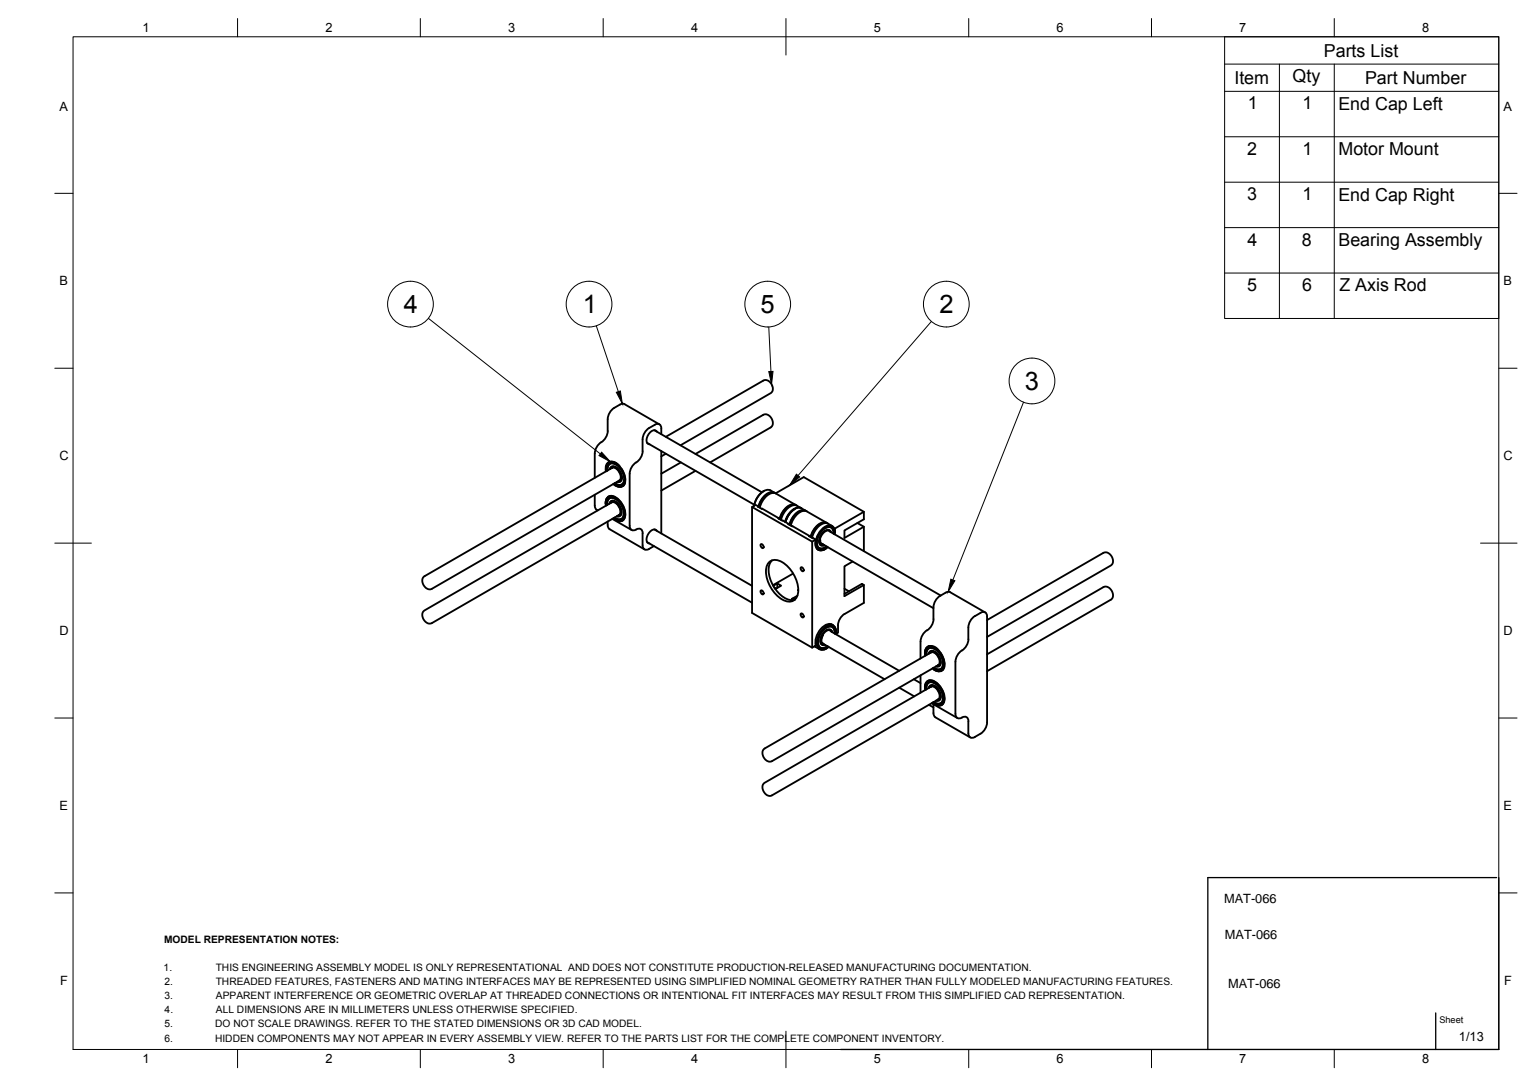
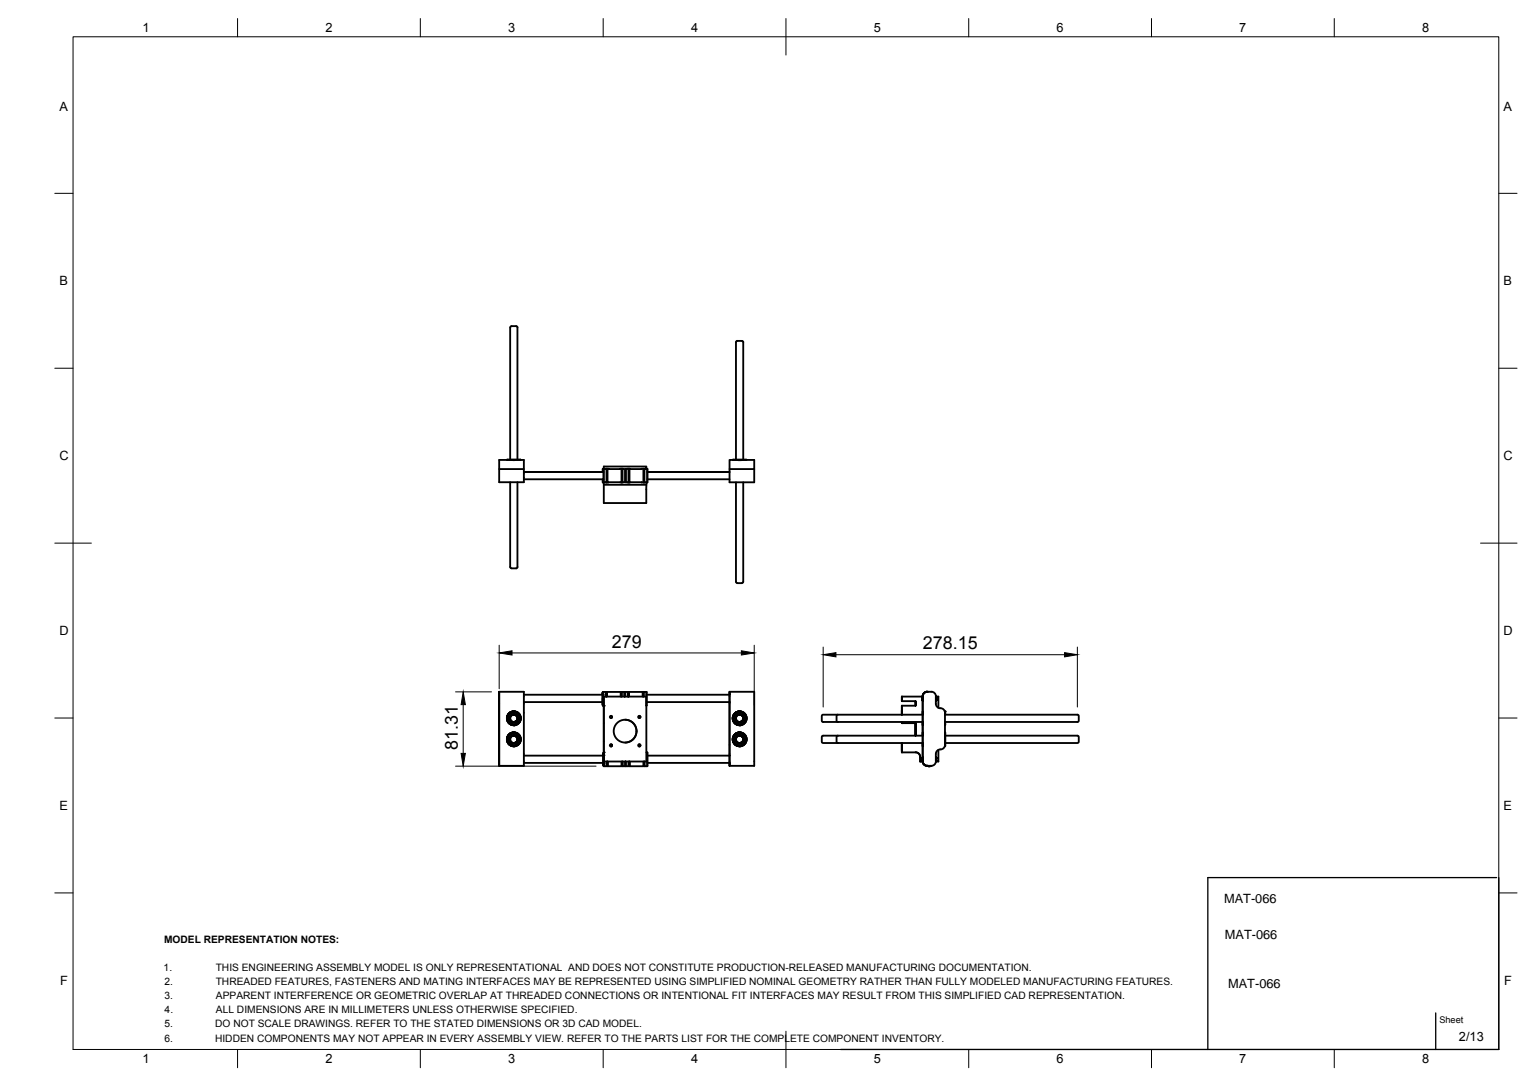
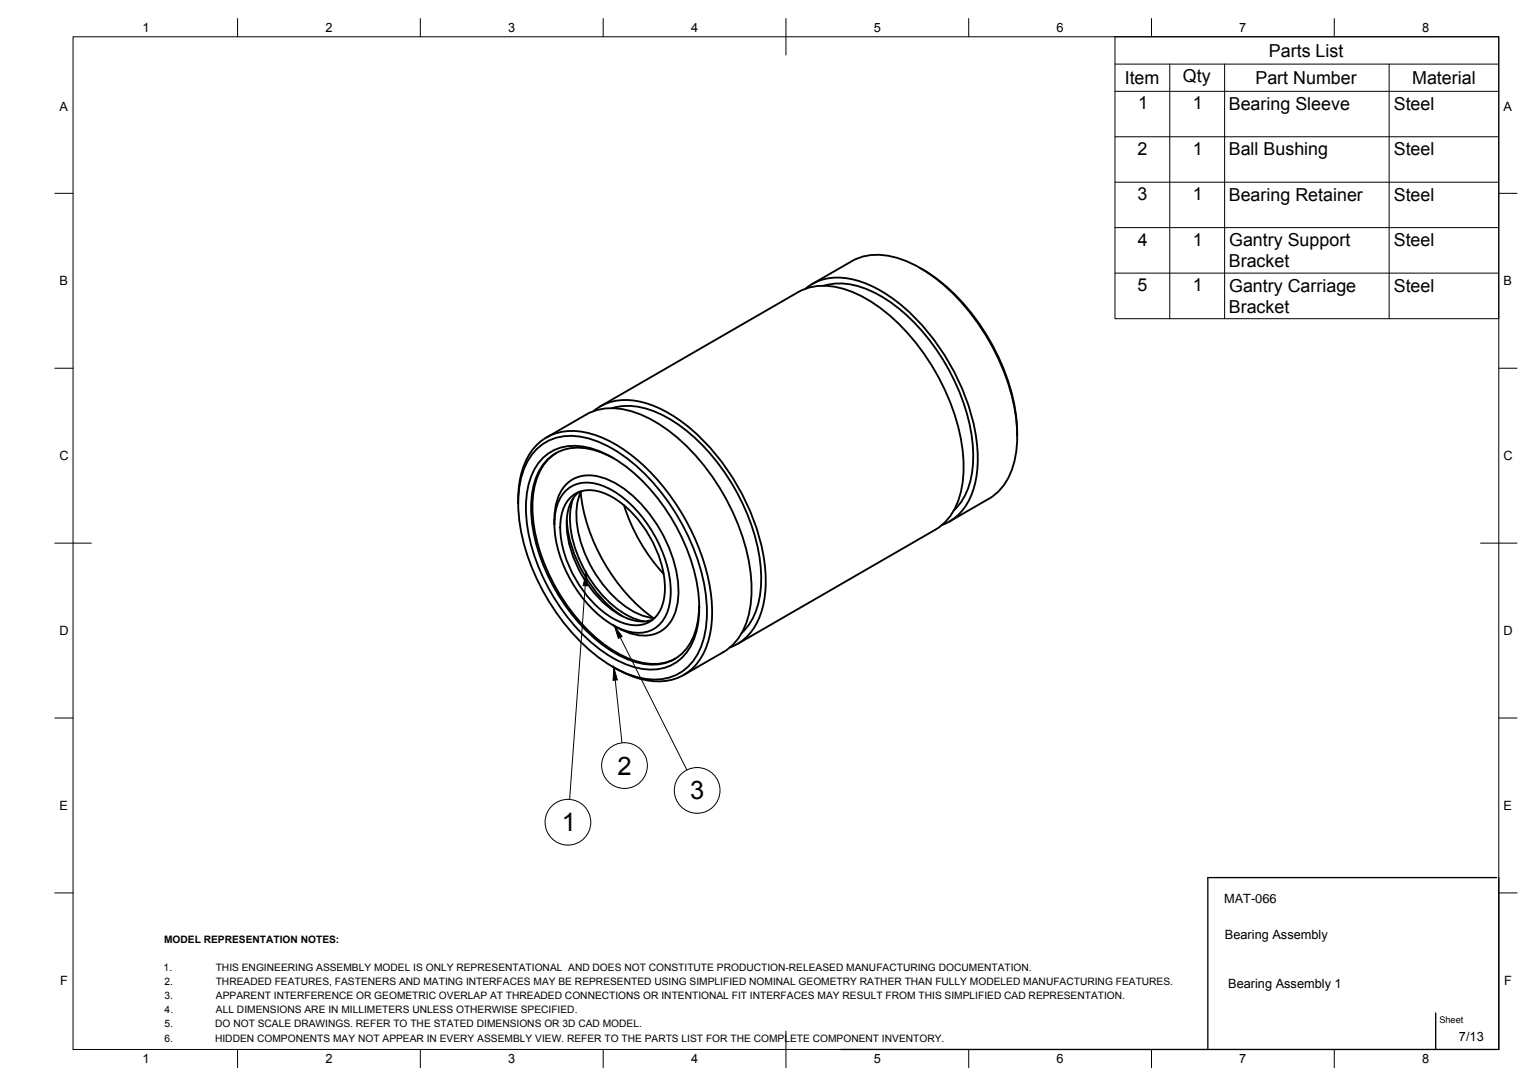
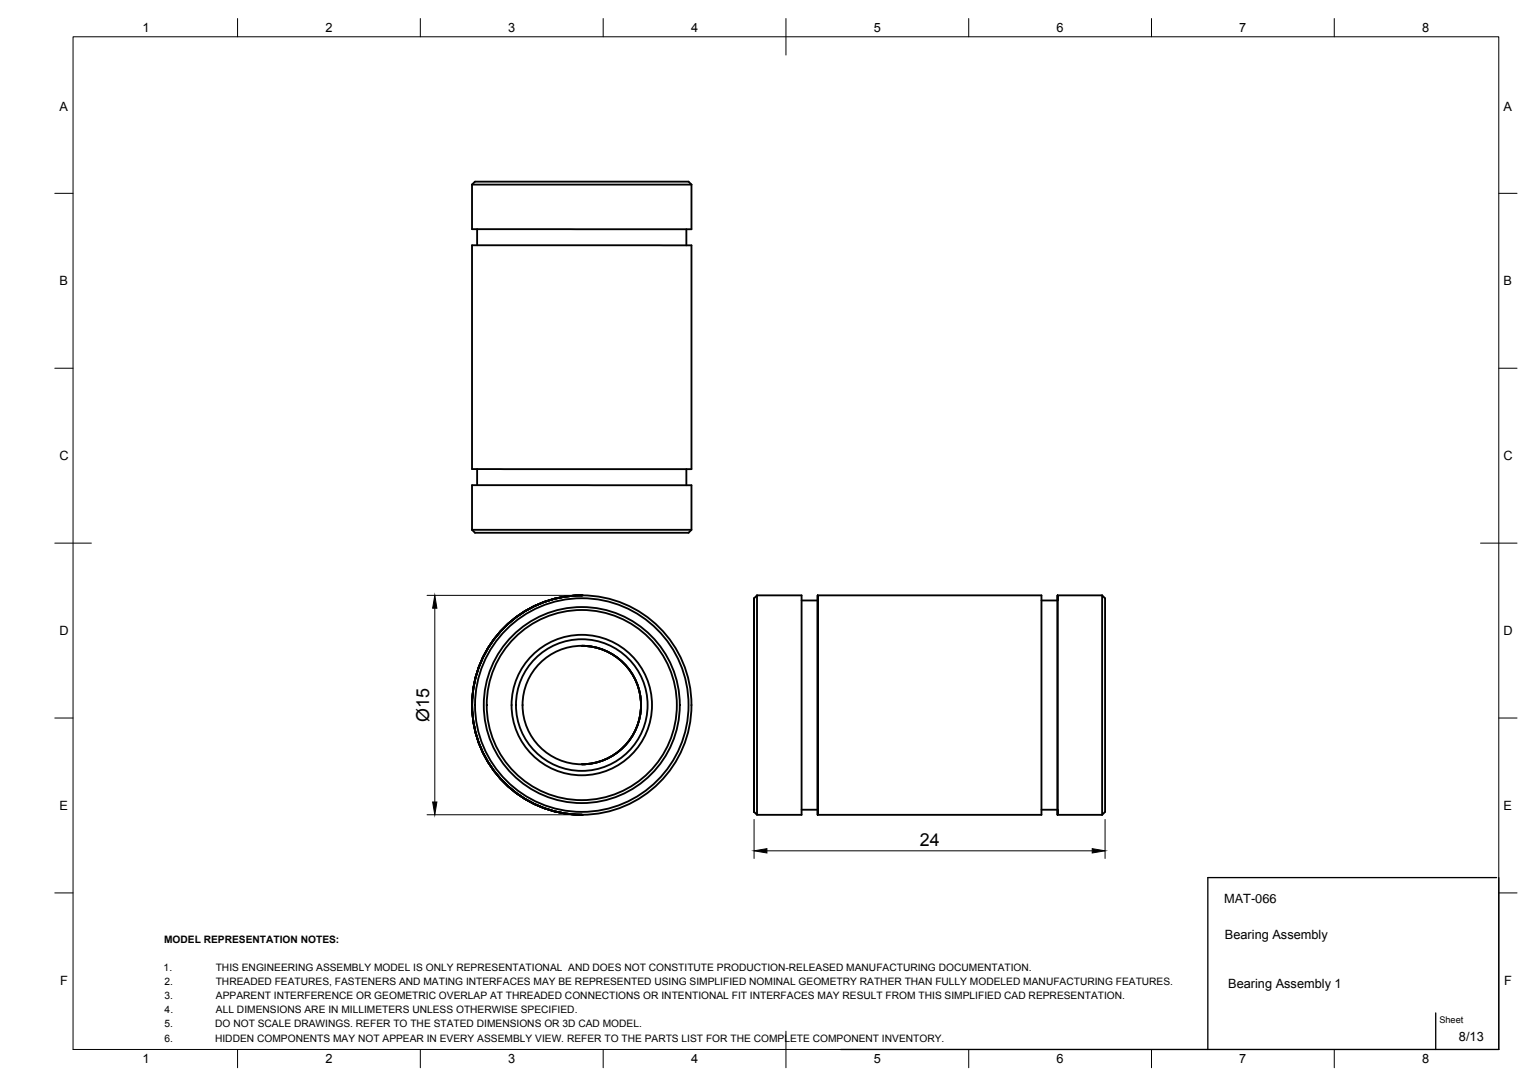
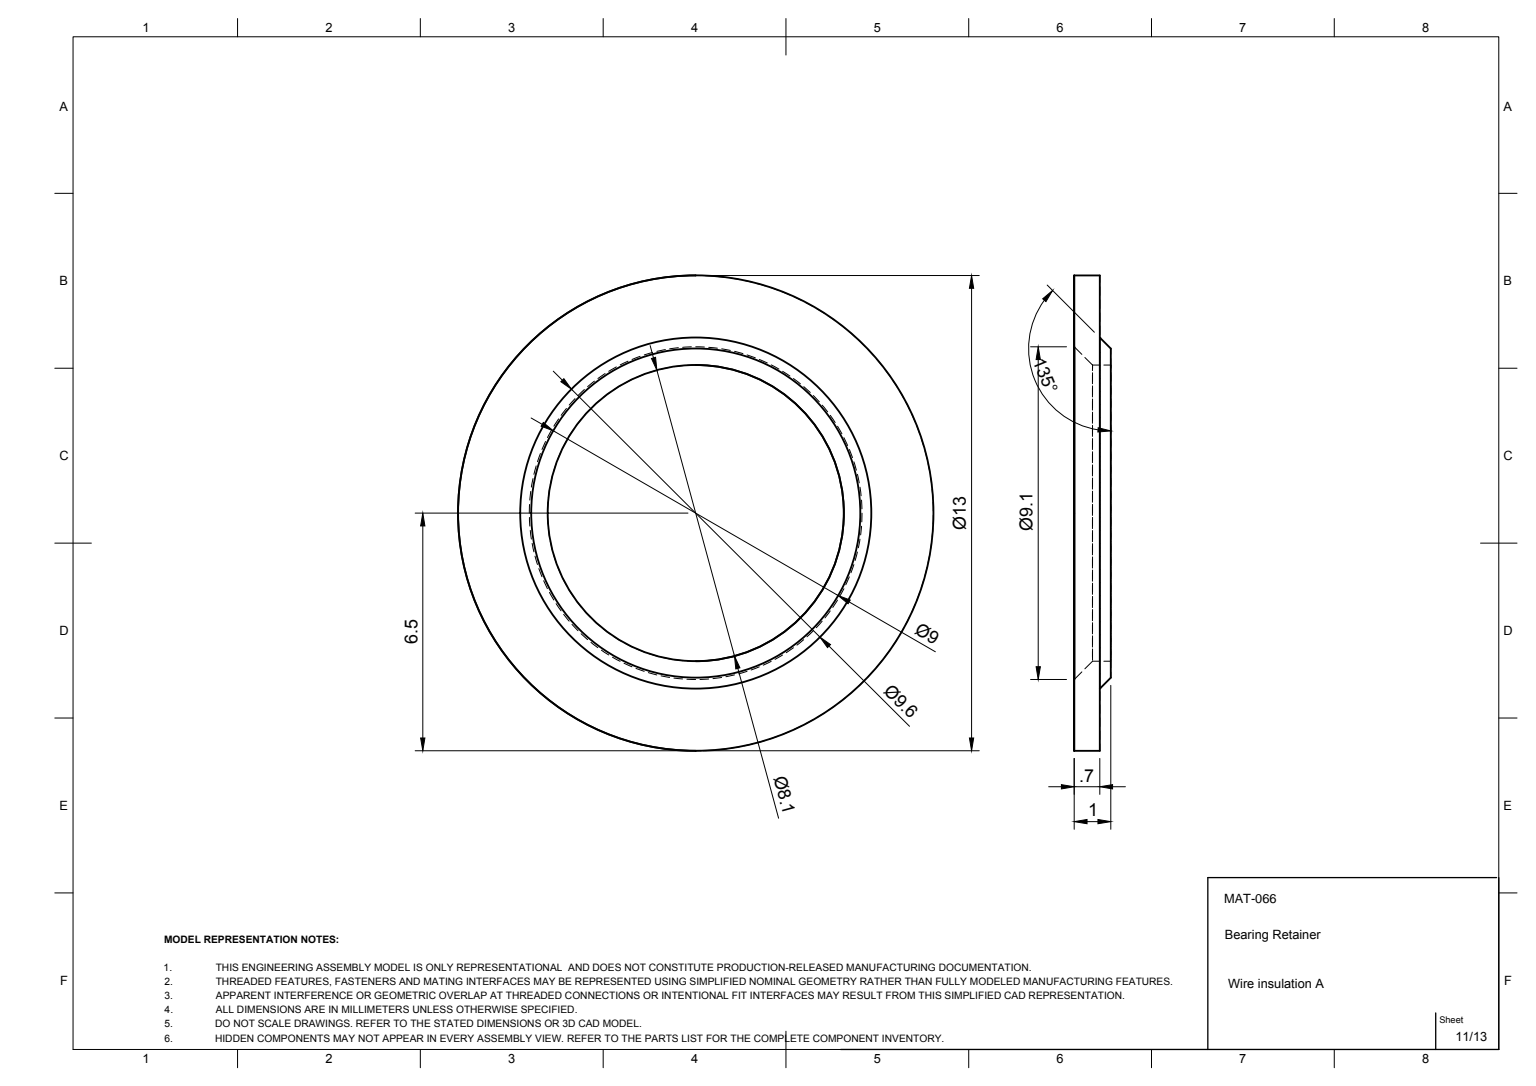
ISO-10303-21;
HEADER;
/* Generated by software containing ST-Developer
 * from STEP Tools, Inc. (www.steptools.com) 
 */

FILE_DESCRIPTION(
/* description */ ('CAx-IF Rec.Pracs.---Representation and Presentation of Product Manufa
cturing Information (PMI)---4.0---2014-10-13'),
/* implementation_level */ '2;1');

FILE_NAME(
/* name */ 'MAT-066',
/* time_stamp */ '2026-10-24T15:58:00-07:00',
/* author */ (''),
/* organization */ (''),
/* preprocessor_version */ 'ST-DEVELOPER v20.2',
/* originating_system */ 'Autodesk Translation Framework v15.17.0.0',
/* authorisation */ '');

FILE_SCHEMA (('AP242_MANAGED_MODEL_BASED_3D_ENGINEERING_MIM_LF { 1 0 10303 442 2 1 4 }'));
ENDSEC;

DATA;
#10=MECHANICAL_DESIGN_GEOMETRIC_PRESENTATION_REPRESENTATION('',(#129,#130,
#131,#132,#133,#134,#135,#136,#137),#8944);
#11=ITEM_DEFINED_TRANSFORMATION($,$,#5686,#5795);
#12=ITEM_DEFINED_TRANSFORMATION($,$,#5695,#5796);
#13=ITEM_DEFINED_TRANSFORMATION($,$,#5756,#5797);
#14=ITEM_DEFINED_TRANSFORMATION($,$,#5771,#5798);
#15=ITEM_DEFINED_TRANSFORMATION($,$,#5780,#5799);
#16=ITEM_DEFINED_TRANSFORMATION($,$,#5260,#5800);
#17=ITEM_DEFINED_TRANSFORMATION($,$,#5308,#5801);
#18=ITEM_DEFINED_TRANSFORMATION($,$,#5623,#5802);
#19=ITEM_DEFINED_TRANSFORMATION($,$,#5685,#5803);
#20=ITEM_DEFINED_TRANSFORMATION($,$,#5671,#5804);
#21=ITEM_DEFINED_TRANSFORMATION($,$,#5671,#5805);
#22=ITEM_DEFINED_TRANSFORMATION($,$,#5671,#5806);
#23=ITEM_DEFINED_TRANSFORMATION($,$,#5671,#5807);
#24=ITEM_DEFINED_TRANSFORMATION($,$,#5671,#5808);
#25=ITEM_DEFINED_TRANSFORMATION($,$,#5671,#5809);
#26=ITEM_DEFINED_TRANSFORMATION($,$,#5685,#5810);
#27=ITEM_DEFINED_TRANSFORMATION($,$,#5685,#5811);
#28=ITEM_DEFINED_TRANSFORMATION($,$,#5685,#5812);
#29=ITEM_DEFINED_TRANSFORMATION($,$,#5685,#5813);
#30=ITEM_DEFINED_TRANSFORMATION($,$,#5685,#5814);
#31=ITEM_DEFINED_TRANSFORMATION($,$,#5685,#5815);
#32=ITEM_DEFINED_TRANSFORMATION($,$,#5685,#5816);
#33=(
REPRESENTATION_RELATIONSHIP($,$,#8998,#8997)
REPRESENTATION_RELATIONSHIP_WITH_TRANSFORMATION(#11)
SHAPE_REPRESENTATION_RELATIONSHIP()
);
#34=(
REPRESENTATION_RELATIONSHIP($,$,#8999,#8997)
REPRESENTATION_RELATIONSHIP_WITH_TRANSFORMATION(#12)
SHAPE_REPRESENTATION_RELATIONSHIP()
);
#35=(
REPRESENTATION_RELATIONSHIP($,$,#9000,#8997)
REPRESENTATION_RELATIONSHIP_WITH_TRANSFORMATION(#13)
SHAPE_REPRESENTATION_RELATIONSHIP()
);
#36=(
REPRESENTATION_RELATIONSHIP($,$,#9001,#8997)
REPRESENTATION_RELATIONSHIP_WITH_TRANSFORMATION(#14)
SHAPE_REPRESENTATION_RELATIONSHIP()
);
#37=(
REPRESENTATION_RELATIONSHIP($,$,#9002,#8997)
REPRESENTATION_RELATIONSHIP_WITH_TRANSFORMATION(#15)
SHAPE_REPRESENTATION_RELATIONSHIP()
);
#38=(
REPRESENTATION_RELATIONSHIP($,$,#8993,#8992)
REPRESENTATION_RELATIONSHIP_WITH_TRANSFORMATION(#16)
SHAPE_REPRESENTATION_RELATIONSHIP()
);
#39=(
REPRESENTATION_RELATIONSHIP($,$,#8994,#8992)
REPRESENTATION_RELATIONSHIP_WITH_TRANSFORMATION(#17)
SHAPE_REPRESENTATION_RELATIONSHIP()
);
#40=(
REPRESENTATION_RELATIONSHIP($,$,#8995,#8992)
REPRESENTATION_RELATIONSHIP_WITH_TRANSFORMATION(#18)
SHAPE_REPRESENTATION_RELATIONSHIP()
);
#41=(
REPRESENTATION_RELATIONSHIP($,$,#8997,#8992)
REPRESENTATION_RELATIONSHIP_WITH_TRANSFORMATION(#19)
SHAPE_REPRESENTATION_RELATIONSHIP()
);
#42=(
REPRESENTATION_RELATIONSHIP($,$,#8996,#8992)
REPRESENTATION_RELATIONSHIP_WITH_TRANSFORMATION(#20)
SHAPE_REPRESENTATION_RELATIONSHIP()
);
#43=(
REPRESENTATION_RELATIONSHIP($,$,#8996,#8992)
REPRESENTATION_RELATIONSHIP_WITH_TRANSFORMATION(#21)
SHAPE_REPRESENTATION_RELATIONSHIP()
);
#44=(
REPRESENTATION_RELATIONSHIP($,$,#8996,#8992)
REPRESENTATION_RELATIONSHIP_WITH_TRANSFORMATION(#22)
SHAPE_REPRESENTATION_RELATIONSHIP()
);
#45=(
REPRESENTATION_RELATIONSHIP($,$,#8996,#8992)
REPRESENTATION_RELATIONSHIP_WITH_TRANSFORMATION(#23)
SHAPE_REPRESENTATION_RELATIONSHIP()
);
#46=(
REPRESENTATION_RELATIONSHIP($,$,#8996,#8992)
REPRESENTATION_RELATIONSHIP_WITH_TRANSFORMATION(#24)
SHAPE_REPRESENTATION_RELATIONSHIP()
);
#47=(
REPRESENTATION_RELATIONSHIP($,$,#8996,#8992)
REPRESENTATION_RELATIONSHIP_WITH_TRANSFORMATION(#25)
SHAPE_REPRESENTATION_RELATIONSHIP()
);
#48=(
REPRESENTATION_RELATIONSHIP($,$,#8997,#8992)
REPRESENTATION_RELATIONSHIP_WITH_TRANSFORMATION(#26)
SHAPE_REPRESENTATION_RELATIONSHIP()
);
#49=(
REPRESENTATION_RELATIONSHIP($,$,#8997,#8992)
REPRESENTATION_RELATIONSHIP_WITH_TRANSFORMATION(#27)
SHAPE_REPRESENTATION_RELATIONSHIP()
);
#50=(
REPRESENTATION_RELATIONSHIP($,$,#8997,#8992)
REPRESENTATION_RELATIONSHIP_WITH_TRANSFORMATION(#28)
SHAPE_REPRESENTATION_RELATIONSHIP()
);
#51=(
REPRESENTATION_RELATIONSHIP($,$,#8997,#8992)
REPRESENTATION_RELATIONSHIP_WITH_TRANSFORMATION(#29)
SHAPE_REPRESENTATION_RELATIONSHIP()
);
#52=(
REPRESENTATION_RELATIONSHIP($,$,#8997,#8992)
REPRESENTATION_RELATIONSHIP_WITH_TRANSFORMATION(#30)
SHAPE_REPRESENTATION_RELATIONSHIP()
);
#53=(
REPRESENTATION_RELATIONSHIP($,$,#8997,#8992)
REPRESENTATION_RELATIONSHIP_WITH_TRANSFORMATION(#31)
SHAPE_REPRESENTATION_RELATIONSHIP()
);
#54=(
REPRESENTATION_RELATIONSHIP($,$,#8997,#8992)
REPRESENTATION_RELATIONSHIP_WITH_TRANSFORMATION(#32)
SHAPE_REPRESENTATION_RELATIONSHIP()
);
#55=CONTEXT_DEPENDENT_SHAPE_REPRESENTATION(#33,#8970);
#56=CONTEXT_DEPENDENT_SHAPE_REPRESENTATION(#34,#8971);
#57=CONTEXT_DEPENDENT_SHAPE_REPRESENTATION(#35,#8972);
#58=CONTEXT_DEPENDENT_SHAPE_REPRESENTATION(#36,#8973);
#59=CONTEXT_DEPENDENT_SHAPE_REPRESENTATION(#37,#8974);
#60=CONTEXT_DEPENDENT_SHAPE_REPRESENTATION(#38,#8975);
#61=CONTEXT_DEPENDENT_SHAPE_REPRESENTATION(#39,#8976);
#62=CONTEXT_DEPENDENT_SHAPE_REPRESENTATION(#40,#8977);
#63=CONTEXT_DEPENDENT_SHAPE_REPRESENTATION(#41,#8978);
#64=CONTEXT_DEPENDENT_SHAPE_REPRESENTATION(#42,#8979);
#65=CONTEXT_DEPENDENT_SHAPE_REPRESENTATION(#43,#8980);
#66=CONTEXT_DEPENDENT_SHAPE_REPRESENTATION(#44,#8981);
#67=CONTEXT_DEPENDENT_SHAPE_REPRESENTATION(#45,#8982);
#68=CONTEXT_DEPENDENT_SHAPE_REPRESENTATION(#46,#8983);
#69=CONTEXT_DEPENDENT_SHAPE_REPRESENTATION(#47,#8984);
#70=CONTEXT_DEPENDENT_SHAPE_REPRESENTATION(#48,#8985);
#71=CONTEXT_DEPENDENT_SHAPE_REPRESENTATION(#49,#8986);
#72=CONTEXT_DEPENDENT_SHAPE_REPRESENTATION(#50,#8987);
#73=CONTEXT_DEPENDENT_SHAPE_REPRESENTATION(#51,#8988);
#74=CONTEXT_DEPENDENT_SHAPE_REPRESENTATION(#52,#8989);
#75=CONTEXT_DEPENDENT_SHAPE_REPRESENTATION(#53,#8990);
#76=CONTEXT_DEPENDENT_SHAPE_REPRESENTATION(#54,#8991);
#77=NEXT_ASSEMBLY_USAGE_OCCURRENCE('Bearing Sleeve:1',
'Bearing Sleeve:1','Bearing Sleeve:1',#9009,#9010,'Bearing Sleeve:1');
#78=NEXT_ASSEMBLY_USAGE_OCCURRENCE('Ball Bushing:1','Ball Bushing:1',
'Ball Bushing:1',#9009,#9011,'Ball Bushing:1');
#79=NEXT_ASSEMBLY_USAGE_OCCURRENCE('Bearing Retainer 1:1',
'Bearing Retainer 1:1','Bearing Retainer 1:1',#9009,#9012,
'Bearing Retainer 1:1');
#80=NEXT_ASSEMBLY_USAGE_OCCURRENCE('Gantry Support Bracket:1',
'Gantry Support Bracket:1','Gantry Support Bracket:1',#9009,#9013,
'Gantry Support Bracket:1');
#81=NEXT_ASSEMBLY_USAGE_OCCURRENCE('Gantry Carriage Bracket:1',
'Gantry Carriage Bracket:1','Gantry Carriage Bracket:1',#9009,#9014,
'Gantry Carriage Bracket:1');
#82=NEXT_ASSEMBLY_USAGE_OCCURRENCE('End Cap Left:1','End Cap Left:1',
'End Cap Left:1',#9004,#9005,'End Cap Left:1');
#83=NEXT_ASSEMBLY_USAGE_OCCURRENCE('Motor Mount:1','Motor Mount:1',
'Motor Mount:1',#9004,#9006,'Motor Mount:1');
#84=NEXT_ASSEMBLY_USAGE_OCCURRENCE('End Cap Right:1','End Cap Right:1',
'End Cap Right:1',#9004,#9007,'End Cap Right:1');
#85=NEXT_ASSEMBLY_USAGE_OCCURRENCE('Bearing Assembly 1:1',
'Bearing Assembly 1:1','Bearing Assembly 1:1',#9004,#9009,
'Bearing Assembly 1:1');
#86=NEXT_ASSEMBLY_USAGE_OCCURRENCE('Z Axis Rod:1','Z Axis Rod:1',
'Z Axis Rod:1',#9004,#9008,'Z Axis Rod:1');
#87=NEXT_ASSEMBLY_USAGE_OCCURRENCE('Z Axis Rod:2','Z Axis Rod:2',
'Z Axis Rod:2',#9004,#9008,'Z Axis Rod:2');
#88=NEXT_ASSEMBLY_USAGE_OCCURRENCE('Z Axis Rod:3','Z Axis Rod:3',
'Z Axis Rod:3',#9004,#9008,'Z Axis Rod:3');
#89=NEXT_ASSEMBLY_USAGE_OCCURRENCE('Z Axis Rod:4','Z Axis Rod:4',
'Z Axis Rod:4',#9004,#9008,'Z Axis Rod:4');
#90=NEXT_ASSEMBLY_USAGE_OCCURRENCE('Z Axis Rod:5','Z Axis Rod:5',
'Z Axis Rod:5',#9004,#9008,'Z Axis Rod:5');
#91=NEXT_ASSEMBLY_USAGE_OCCURRENCE('Z Axis Rod:6','Z Axis Rod:6',
'Z Axis Rod:6',#9004,#9008,'Z Axis Rod:6');
#92=NEXT_ASSEMBLY_USAGE_OCCURRENCE('Bearing Assembly 1:2',
'Bearing Assembly 1:2','Bearing Assembly 1:2',#9004,#9009,
'Bearing Assembly 1:2');
#93=NEXT_ASSEMBLY_USAGE_OCCURRENCE('Bearing Assembly 1:3',
'Bearing Assembly 1:3','Bearing Assembly 1:3',#9004,#9009,
'Bearing Assembly 1:3');
#94=NEXT_ASSEMBLY_USAGE_OCCURRENCE('Bearing Assembly 1:4',
'Bearing Assembly 1:4','Bearing Assembly 1:4',#9004,#9009,
'Bearing Assembly 1:4');
#95=NEXT_ASSEMBLY_USAGE_OCCURRENCE('Bearing Assembly 1:5',
'Bearing Assembly 1:5','Bearing Assembly 1:5',#9004,#9009,
'Bearing Assembly 1:5');
#96=NEXT_ASSEMBLY_USAGE_OCCURRENCE('Bearing Assembly 1:6',
'Bearing Assembly 1:6','Bearing Assembly 1:6',#9004,#9009,
'Bearing Assembly 1:6');
#97=NEXT_ASSEMBLY_USAGE_OCCURRENCE('Bearing Assembly 1:7',
'Bearing Assembly 1:7','Bearing Assembly 1:7',#9004,#9009,
'Bearing Assembly 1:7');
#98=NEXT_ASSEMBLY_USAGE_OCCURRENCE('Bearing Assembly 1:8',
'Bearing Assembly 1:8','Bearing Assembly 1:8',#9004,#9009,
'Bearing Assembly 1:8');
#99=CONICAL_SURFACE('',#5696,0.0066,0.785398163397459);
#100=CONICAL_SURFACE('',#5704,0.0074,0.785398163397448);
#101=CONICAL_SURFACE('',#5709,0.0066,0.785398163397459);
#102=CONICAL_SURFACE('',#5717,0.0074,0.785398163397448);
#103=CONICAL_SURFACE('',#5730,0.0061,0.158655262186402);
#104=CONICAL_SURFACE('',#5734,0.0061,0.158655262186402);
#105=CONICAL_SURFACE('',#5764,0.0043,0.785398163397448);
#106=CONICAL_SURFACE('',#5770,0.0046499998960644,0.785398163397448);
#107=CONICAL_SURFACE('',#5788,0.0043,0.785398163397448);
#108=CONICAL_SURFACE('',#5794,0.0046499998960644,0.785398163397448);
#109=TOROIDAL_SURFACE('',#5681,0.0025,0.0015);
#110=TOROIDAL_SURFACE('',#5683,0.0025,0.0015);
#111=SHAPE_REPRESENTATION_RELATIONSHIP('SRR','None',#8993,#120);
#112=SHAPE_REPRESENTATION_RELATIONSHIP('SRR','None',#8994,#121);
#113=SHAPE_REPRESENTATION_RELATIONSHIP('SRR','None',#8995,#122);
#114=SHAPE_REPRESENTATION_RELATIONSHIP('SRR','None',#8996,#123);
#115=SHAPE_REPRESENTATION_RELATIONSHIP('SRR','None',#8998,#124);
#116=SHAPE_REPRESENTATION_RELATIONSHIP('SRR','None',#8999,#125);
#117=SHAPE_REPRESENTATION_RELATIONSHIP('SRR','None',#9000,#126);
#118=SHAPE_REPRESENTATION_RELATIONSHIP('SRR','None',#9001,#127);
#119=SHAPE_REPRESENTATION_RELATIONSHIP('SRR','None',#9002,#128);
#120=ADVANCED_BREP_SHAPE_REPRESENTATION('',(#138),#8934);
#121=ADVANCED_BREP_SHAPE_REPRESENTATION('',(#139),#8935);
#122=ADVANCED_BREP_SHAPE_REPRESENTATION('',(#140),#8936);
#123=ADVANCED_BREP_SHAPE_REPRESENTATION('',(#141),#8937);
#124=ADVANCED_BREP_SHAPE_REPRESENTATION('',(#142),#8939);
#125=ADVANCED_BREP_SHAPE_REPRESENTATION('',(#143),#8940);
#126=ADVANCED_BREP_SHAPE_REPRESENTATION('',(#144),#8941);
#127=ADVANCED_BREP_SHAPE_REPRESENTATION('',(#145),#8942);
#128=ADVANCED_BREP_SHAPE_REPRESENTATION('',(#146),#8943);
#129=STYLED_ITEM('',(#9052),#138);
#130=STYLED_ITEM('',(#9053),#139);
#131=STYLED_ITEM('',(#9054),#140);
#132=STYLED_ITEM('',(#9055),#141);
#133=STYLED_ITEM('',(#9052),#142);
#134=STYLED_ITEM('',(#9054),#143);
#135=STYLED_ITEM('',(#9052),#144);
#136=STYLED_ITEM('',(#9054),#145);
#137=STYLED_ITEM('',(#9052),#146);
#138=MANIFOLD_SOLID_BREP('Body1',#5150);
#139=MANIFOLD_SOLID_BREP('Body1',#5151);
#140=MANIFOLD_SOLID_BREP('Body1',#5152);
#141=MANIFOLD_SOLID_BREP('Body1',#5153);
#142=MANIFOLD_SOLID_BREP('Body1',#5154);
#143=MANIFOLD_SOLID_BREP('Body1',#5155);
#144=MANIFOLD_SOLID_BREP('Body1',#5156);
#145=MANIFOLD_SOLID_BREP('Body1',#5157);
#146=MANIFOLD_SOLID_BREP('Body1',#5158);
#147=B_SPLINE_CURVE_WITH_KNOTS('',3,(#7501,#7502,#7503,#7504,#7505,#7506),
 .UNSPECIFIED.,.F.,.F.,(4,2,4),(3.46797062946804,3.66737221611079,3.95578831781598),
 .UNSPECIFIED.);
#148=B_SPLINE_CURVE_WITH_KNOTS('',3,(#7507,#7508,#7509,#7510,#7511,#7512),
 .UNSPECIFIED.,.F.,.F.,(4,2,4),(3.95578831781598,4.24420441952117,4.44360600616391),
 .UNSPECIFIED.);
#149=B_SPLINE_CURVE_WITH_KNOTS('',3,(#7515,#7516,#7517,#7518,#7519,#7520,
#7521,#7522,#7523,#7524),.UNSPECIFIED.,.F.,.F.,(4,2,2,2,4),(-4.44360600616391,
-4.24420441952117,-3.95578831781597,-3.66737221611078,-3.46797062946804),
 .UNSPECIFIED.);
#150=B_SPLINE_CURVE_WITH_KNOTS('',3,(#8654,#8655,#8656,#8657,#8658,#8659),
 .UNSPECIFIED.,.F.,.F.,(4,2,4),(3.46797062946804,3.66737221611079,3.95578831781598),
 .UNSPECIFIED.);
#151=B_SPLINE_CURVE_WITH_KNOTS('',3,(#8660,#8661,#8662,#8663,#8664,#8665),
 .UNSPECIFIED.,.F.,.F.,(4,2,4),(3.95578831781598,4.24420441952117,4.44360600616391),
 .UNSPECIFIED.);
#152=B_SPLINE_CURVE_WITH_KNOTS('',3,(#8668,#8669,#8670,#8671,#8672,#8673,
#8674,#8675,#8676,#8677),.UNSPECIFIED.,.F.,.F.,(4,2,2,2,4),(3.46797062946804,
3.66737221611078,3.95578831781597,4.24420441952117,4.44360600616391),
 .UNSPECIFIED.);
#153=CYLINDRICAL_SURFACE('',#5276,0.004225);
#154=CYLINDRICAL_SURFACE('',#5280,0.004225);
#155=CYLINDRICAL_SURFACE('',#5294,0.005);
#156=CYLINDRICAL_SURFACE('',#5295,0.005);
#157=CYLINDRICAL_SURFACE('',#5296,0.005);
#158=CYLINDRICAL_SURFACE('',#5297,0.005);
#159=CYLINDRICAL_SURFACE('',#5302,0.007625);
#160=CYLINDRICAL_SURFACE('',#5303,0.007625);
#161=CYLINDRICAL_SURFACE('',#5304,0.005);
#162=CYLINDRICAL_SURFACE('',#5305,0.005);
#163=CYLINDRICAL_SURFACE('',#5306,0.005);
#164=CYLINDRICAL_SURFACE('',#5307,0.005);
#165=CYLINDRICAL_SURFACE('',#5384,0.0125);
#166=CYLINDRICAL_SURFACE('',#5385,0.00123);
#167=CYLINDRICAL_SURFACE('',#5386,0.00123);
#168=CYLINDRICAL_SURFACE('',#5387,0.00123);
#169=CYLINDRICAL_SURFACE('',#5388,0.00123);
#170=CYLINDRICAL_SURFACE('',#5414,0.0076);
#171=CYLINDRICAL_SURFACE('',#5487,0.0023);
#172=CYLINDRICAL_SURFACE('',#5488,0.0023);
#173=CYLINDRICAL_SURFACE('',#5489,0.0023);
#174=CYLINDRICAL_SURFACE('',#5490,0.0023);
#175=CYLINDRICAL_SURFACE('',#5491,0.0023);
#176=CYLINDRICAL_SURFACE('',#5492,0.0023);
#177=CYLINDRICAL_SURFACE('',#5493,0.0023);
#178=CYLINDRICAL_SURFACE('',#5494,0.0023);
#179=CYLINDRICAL_SURFACE('',#5495,0.0023);
#180=CYLINDRICAL_SURFACE('',#5496,0.0023);
#181=CYLINDRICAL_SURFACE('',#5497,0.0023);
#182=CYLINDRICAL_SURFACE('',#5498,0.0023);
#183=CYLINDRICAL_SURFACE('',#5499,0.0023);
#184=CYLINDRICAL_SURFACE('',#5500,0.0023);
#185=CYLINDRICAL_SURFACE('',#5501,0.0023);
#186=CYLINDRICAL_SURFACE('',#5502,0.0023);
#187=CYLINDRICAL_SURFACE('',#5525,0.0076);
#188=CYLINDRICAL_SURFACE('',#5606,0.0023);
#189=CYLINDRICAL_SURFACE('',#5607,0.0023);
#190=CYLINDRICAL_SURFACE('',#5608,0.0023);
#191=CYLINDRICAL_SURFACE('',#5609,0.0023);
#192=CYLINDRICAL_SURFACE('',#5610,0.0023);
#193=CYLINDRICAL_SURFACE('',#5611,0.0023);
#194=CYLINDRICAL_SURFACE('',#5612,0.0023);
#195=CYLINDRICAL_SURFACE('',#5613,0.0023);
#196=CYLINDRICAL_SURFACE('',#5614,0.0023);
#197=CYLINDRICAL_SURFACE('',#5615,0.0023);
#198=CYLINDRICAL_SURFACE('',#5616,0.0023);
#199=CYLINDRICAL_SURFACE('',#5617,0.0023);
#200=CYLINDRICAL_SURFACE('',#5618,0.0023);
#201=CYLINDRICAL_SURFACE('',#5619,0.0023);
#202=CYLINDRICAL_SURFACE('',#5620,0.0023);
#203=CYLINDRICAL_SURFACE('',#5621,0.0023);
#204=CYLINDRICAL_SURFACE('',#5622,0.005);
#205=CYLINDRICAL_SURFACE('',#5639,0.004225);
#206=CYLINDRICAL_SURFACE('',#5643,0.004225);
#207=CYLINDRICAL_SURFACE('',#5657,0.005);
#208=CYLINDRICAL_SURFACE('',#5658,0.005);
#209=CYLINDRICAL_SURFACE('',#5659,0.005);
#210=CYLINDRICAL_SURFACE('',#5660,0.005);
#211=CYLINDRICAL_SURFACE('',#5665,0.007625);
#212=CYLINDRICAL_SURFACE('',#5666,0.007625);
#213=CYLINDRICAL_SURFACE('',#5667,0.005);
#214=CYLINDRICAL_SURFACE('',#5668,0.005);
#215=CYLINDRICAL_SURFACE('',#5669,0.005);
#216=CYLINDRICAL_SURFACE('',#5670,0.005);
#217=CYLINDRICAL_SURFACE('',#5672,0.004);
#218=CYLINDRICAL_SURFACE('',#5690,0.007);
#219=CYLINDRICAL_SURFACE('',#5694,0.0043);
#220=CYLINDRICAL_SURFACE('',#5702,0.0065);
#221=CYLINDRICAL_SURFACE('',#5707,0.0075);
#222=CYLINDRICAL_SURFACE('',#5715,0.0065);
#223=CYLINDRICAL_SURFACE('',#5720,0.0075);
#224=CYLINDRICAL_SURFACE('',#5724,0.00700000010430813);
#225=CYLINDRICAL_SURFACE('',#5728,0.0063);
#226=CYLINDRICAL_SURFACE('',#5732,0.0059);
#227=CYLINDRICAL_SURFACE('',#5736,0.0063);
#228=CYLINDRICAL_SURFACE('',#5740,0.00700000010430813);
#229=CYLINDRICAL_SURFACE('',#5745,0.00715);
#230=CYLINDRICAL_SURFACE('',#5749,0.0075);
#231=CYLINDRICAL_SURFACE('',#5753,0.00715);
#232=CYLINDRICAL_SURFACE('',#5760,0.0065);
#233=CYLINDRICAL_SURFACE('',#5766,0.00405);
#234=CYLINDRICAL_SURFACE('',#5775,0.007);
#235=CYLINDRICAL_SURFACE('',#5779,0.0043);
#236=CYLINDRICAL_SURFACE('',#5784,0.0065);
#237=CYLINDRICAL_SURFACE('',#5790,0.00405);
#238=FACE_BOUND('',#581,.T.);
#239=FACE_BOUND('',#582,.T.);
#240=FACE_BOUND('',#588,.T.);
#241=FACE_BOUND('',#589,.T.);
#242=FACE_BOUND('',#613,.T.);
#243=FACE_BOUND('',#614,.T.);
#244=FACE_BOUND('',#615,.T.);
#245=FACE_BOUND('',#616,.T.);
#246=FACE_BOUND('',#617,.T.);
#247=FACE_BOUND('',#618,.T.);
#248=FACE_BOUND('',#619,.T.);
#249=FACE_BOUND('',#620,.T.);
#250=FACE_BOUND('',#634,.T.);
#251=FACE_BOUND('',#635,.T.);
#252=FACE_BOUND('',#636,.T.);
#253=FACE_BOUND('',#637,.T.);
#254=FACE_BOUND('',#638,.T.);
#255=FACE_BOUND('',#639,.T.);
#256=FACE_BOUND('',#640,.T.);
#257=FACE_BOUND('',#641,.T.);
#258=FACE_BOUND('',#659,.T.);
#259=FACE_BOUND('',#660,.T.);
#260=FACE_BOUND('',#661,.T.);
#261=FACE_BOUND('',#662,.T.);
#262=FACE_BOUND('',#663,.T.);
#263=FACE_BOUND('',#666,.T.);
#264=FACE_BOUND('',#667,.T.);
#265=FACE_BOUND('',#668,.T.);
#266=FACE_BOUND('',#669,.T.);
#267=FACE_BOUND('',#670,.T.);
#268=FACE_BOUND('',#694,.T.);
#269=FACE_BOUND('',#695,.T.);
#270=FACE_BOUND('',#696,.T.);
#271=FACE_BOUND('',#697,.T.);
#272=FACE_BOUND('',#698,.T.);
#273=FACE_BOUND('',#699,.T.);
#274=FACE_BOUND('',#700,.T.);
#275=FACE_BOUND('',#701,.T.);
#276=FACE_BOUND('',#758,.T.);
#277=FACE_BOUND('',#759,.T.);
#278=FACE_BOUND('',#760,.T.);
#279=FACE_BOUND('',#761,.T.);
#280=FACE_BOUND('',#762,.T.);
#281=FACE_BOUND('',#763,.T.);
#282=FACE_BOUND('',#764,.T.);
#283=FACE_BOUND('',#765,.T.);
#284=FACE_BOUND('',#819,.T.);
#285=FACE_BOUND('',#820,.T.);
#286=FACE_BOUND('',#826,.T.);
#287=FACE_BOUND('',#827,.T.);
#288=FACE_BOUND('',#847,.T.);
#289=FACE_BOUND('',#850,.T.);
#290=FACE_BOUND('',#854,.T.);
#291=FACE_BOUND('',#860,.T.);
#292=FACE_BOUND('',#865,.T.);
#293=FACE_BOUND('',#868,.T.);
#294=FACE_BOUND('',#875,.T.);
#295=FACE_BOUND('',#878,.T.);
#296=FACE_BOUND('',#880,.T.);
#297=FACE_BOUND('',#883,.T.);
#298=FACE_BOUND('',#886,.T.);
#299=FACE_BOUND('',#889,.T.);
#300=FACE_BOUND('',#891,.T.);
#301=FACE_BOUND('',#894,.T.);
#302=FACE_BOUND('',#898,.T.);
#303=FACE_BOUND('',#901,.T.);
#304=FACE_BOUND('',#904,.T.);
#305=FACE_BOUND('',#907,.T.);
#306=FACE_BOUND('',#910,.T.);
#307=FACE_BOUND('',#914,.T.);
#308=FACE_OUTER_BOUND('',#577,.T.);
#309=FACE_OUTER_BOUND('',#578,.T.);
#310=FACE_OUTER_BOUND('',#579,.T.);
#311=FACE_OUTER_BOUND('',#580,.T.);
#312=FACE_OUTER_BOUND('',#583,.T.);
#313=FACE_OUTER_BOUND('',#584,.T.);
#314=FACE_OUTER_BOUND('',#585,.T.);
#315=FACE_OUTER_BOUND('',#586,.T.);
#316=FACE_OUTER_BOUND('',#587,.T.);
#317=FACE_OUTER_BOUND('',#590,.T.);
#318=FACE_OUTER_BOUND('',#591,.T.);
#319=FACE_OUTER_BOUND('',#592,.T.);
#320=FACE_OUTER_BOUND('',#593,.T.);
#321=FACE_OUTER_BOUND('',#594,.T.);
#322=FACE_OUTER_BOUND('',#595,.T.);
#323=FACE_OUTER_BOUND('',#596,.T.);
#324=FACE_OUTER_BOUND('',#597,.T.);
#325=FACE_OUTER_BOUND('',#598,.T.);
#326=FACE_OUTER_BOUND('',#599,.T.);
#327=FACE_OUTER_BOUND('',#600,.T.);
#328=FACE_OUTER_BOUND('',#601,.T.);
#329=FACE_OUTER_BOUND('',#602,.T.);
#330=FACE_OUTER_BOUND('',#603,.T.);
#331=FACE_OUTER_BOUND('',#604,.T.);
#332=FACE_OUTER_BOUND('',#605,.T.);
#333=FACE_OUTER_BOUND('',#606,.T.);
#334=FACE_OUTER_BOUND('',#607,.T.);
#335=FACE_OUTER_BOUND('',#608,.T.);
#336=FACE_OUTER_BOUND('',#609,.T.);
#337=FACE_OUTER_BOUND('',#610,.T.);
#338=FACE_OUTER_BOUND('',#611,.T.);
#339=FACE_OUTER_BOUND('',#612,.T.);
#340=FACE_OUTER_BOUND('',#621,.T.);
#341=FACE_OUTER_BOUND('',#622,.T.);
#342=FACE_OUTER_BOUND('',#623,.T.);
#343=FACE_OUTER_BOUND('',#624,.T.);
#344=FACE_OUTER_BOUND('',#625,.T.);
#345=FACE_OUTER_BOUND('',#626,.T.);
#346=FACE_OUTER_BOUND('',#627,.T.);
#347=FACE_OUTER_BOUND('',#628,.T.);
#348=FACE_OUTER_BOUND('',#629,.T.);
#349=FACE_OUTER_BOUND('',#630,.T.);
#350=FACE_OUTER_BOUND('',#631,.T.);
#351=FACE_OUTER_BOUND('',#632,.T.);
#352=FACE_OUTER_BOUND('',#633,.T.);
#353=FACE_OUTER_BOUND('',#642,.T.);
#354=FACE_OUTER_BOUND('',#643,.T.);
#355=FACE_OUTER_BOUND('',#644,.T.);
#356=FACE_OUTER_BOUND('',#645,.T.);
#357=FACE_OUTER_BOUND('',#646,.T.);
#358=FACE_OUTER_BOUND('',#647,.T.);
#359=FACE_OUTER_BOUND('',#648,.T.);
#360=FACE_OUTER_BOUND('',#649,.T.);
#361=FACE_OUTER_BOUND('',#650,.T.);
#362=FACE_OUTER_BOUND('',#651,.T.);
#363=FACE_OUTER_BOUND('',#652,.T.);
#364=FACE_OUTER_BOUND('',#653,.T.);
#365=FACE_OUTER_BOUND('',#654,.T.);
#366=FACE_OUTER_BOUND('',#655,.T.);
#367=FACE_OUTER_BOUND('',#656,.T.);
#368=FACE_OUTER_BOUND('',#657,.T.);
#369=FACE_OUTER_BOUND('',#658,.T.);
#370=FACE_OUTER_BOUND('',#664,.T.);
#371=FACE_OUTER_BOUND('',#665,.T.);
#372=FACE_OUTER_BOUND('',#671,.T.);
#373=FACE_OUTER_BOUND('',#672,.T.);
#374=FACE_OUTER_BOUND('',#673,.T.);
#375=FACE_OUTER_BOUND('',#674,.T.);
#376=FACE_OUTER_BOUND('',#675,.T.);
#377=FACE_OUTER_BOUND('',#676,.T.);
#378=FACE_OUTER_BOUND('',#677,.T.);
#379=FACE_OUTER_BOUND('',#678,.T.);
#380=FACE_OUTER_BOUND('',#679,.T.);
#381=FACE_OUTER_BOUND('',#680,.T.);
#382=FACE_OUTER_BOUND('',#681,.T.);
#383=FACE_OUTER_BOUND('',#682,.T.);
#384=FACE_OUTER_BOUND('',#683,.T.);
#385=FACE_OUTER_BOUND('',#684,.T.);
#386=FACE_OUTER_BOUND('',#685,.T.);
#387=FACE_OUTER_BOUND('',#686,.T.);
#388=FACE_OUTER_BOUND('',#687,.T.);
#389=FACE_OUTER_BOUND('',#688,.T.);
#390=FACE_OUTER_BOUND('',#689,.T.);
#391=FACE_OUTER_BOUND('',#690,.T.);
#392=FACE_OUTER_BOUND('',#691,.T.);
#393=FACE_OUTER_BOUND('',#692,.T.);
#394=FACE_OUTER_BOUND('',#693,.T.);
#395=FACE_OUTER_BOUND('',#702,.T.);
#396=FACE_OUTER_BOUND('',#703,.T.);
#397=FACE_OUTER_BOUND('',#704,.T.);
#398=FACE_OUTER_BOUND('',#705,.T.);
#399=FACE_OUTER_BOUND('',#706,.T.);
#400=FACE_OUTER_BOUND('',#707,.T.);
#401=FACE_OUTER_BOUND('',#708,.T.);
#402=FACE_OUTER_BOUND('',#709,.T.);
#403=FACE_OUTER_BOUND('',#710,.T.);
#404=FACE_OUTER_BOUND('',#711,.T.);
#405=FACE_OUTER_BOUND('',#712,.T.);
#406=FACE_OUTER_BOUND('',#713,.T.);
#407=FACE_OUTER_BOUND('',#714,.T.);
#408=FACE_OUTER_BOUND('',#715,.T.);
#409=FACE_OUTER_BOUND('',#716,.T.);
#410=FACE_OUTER_BOUND('',#717,.T.);
#411=FACE_OUTER_BOUND('',#718,.T.);
#412=FACE_OUTER_BOUND('',#719,.T.);
#413=FACE_OUTER_BOUND('',#720,.T.);
#414=FACE_OUTER_BOUND('',#721,.T.);
#415=FACE_OUTER_BOUND('',#722,.T.);
#416=FACE_OUTER_BOUND('',#723,.T.);
#417=FACE_OUTER_BOUND('',#724,.T.);
#418=FACE_OUTER_BOUND('',#725,.T.);
#419=FACE_OUTER_BOUND('',#726,.T.);
#420=FACE_OUTER_BOUND('',#727,.T.);
#421=FACE_OUTER_BOUND('',#728,.T.);
#422=FACE_OUTER_BOUND('',#729,.T.);
#423=FACE_OUTER_BOUND('',#730,.T.);
#424=FACE_OUTER_BOUND('',#731,.T.);
#425=FACE_OUTER_BOUND('',#732,.T.);
#426=FACE_OUTER_BOUND('',#733,.T.);
#427=FACE_OUTER_BOUND('',#734,.T.);
#428=FACE_OUTER_BOUND('',#735,.T.);
#429=FACE_OUTER_BOUND('',#736,.T.);
#430=FACE_OUTER_BOUND('',#737,.T.);
#431=FACE_OUTER_BOUND('',#738,.T.);
#432=FACE_OUTER_BOUND('',#739,.T.);
#433=FACE_OUTER_BOUND('',#740,.T.);
#434=FACE_OUTER_BOUND('',#741,.T.);
#435=FACE_OUTER_BOUND('',#742,.T.);
#436=FACE_OUTER_BOUND('',#743,.T.);
#437=FACE_OUTER_BOUND('',#744,.T.);
#438=FACE_OUTER_BOUND('',#745,.T.);
#439=FACE_OUTER_BOUND('',#746,.T.);
#440=FACE_OUTER_BOUND('',#747,.T.);
#441=FACE_OUTER_BOUND('',#748,.T.);
#442=FACE_OUTER_BOUND('',#749,.T.);
#443=FACE_OUTER_BOUND('',#750,.T.);
#444=FACE_OUTER_BOUND('',#751,.T.);
#445=FACE_OUTER_BOUND('',#752,.T.);
#446=FACE_OUTER_BOUND('',#753,.T.);
#447=FACE_OUTER_BOUND('',#754,.T.);
#448=FACE_OUTER_BOUND('',#755,.T.);
#449=FACE_OUTER_BOUND('',#756,.T.);
#450=FACE_OUTER_BOUND('',#757,.T.);
#451=FACE_OUTER_BOUND('',#766,.T.);
#452=FACE_OUTER_BOUND('',#767,.T.);
#453=FACE_OUTER_BOUND('',#768,.T.);
#454=FACE_OUTER_BOUND('',#769,.T.);
#455=FACE_OUTER_BOUND('',#770,.T.);
#456=FACE_OUTER_BOUND('',#771,.T.);
#457=FACE_OUTER_BOUND('',#772,.T.);
#458=FACE_OUTER_BOUND('',#773,.T.);
#459=FACE_OUTER_BOUND('',#774,.T.);
#460=FACE_OUTER_BOUND('',#775,.T.);
#461=FACE_OUTER_BOUND('',#776,.T.);
#462=FACE_OUTER_BOUND('',#777,.T.);
#463=FACE_OUTER_BOUND('',#778,.T.);
#464=FACE_OUTER_BOUND('',#779,.T.);
#465=FACE_OUTER_BOUND('',#780,.T.);
#466=FACE_OUTER_BOUND('',#781,.T.);
#467=FACE_OUTER_BOUND('',#782,.T.);
#468=FACE_OUTER_BOUND('',#783,.T.);
#469=FACE_OUTER_BOUND('',#784,.T.);
#470=FACE_OUTER_BOUND('',#785,.T.);
#471=FACE_OUTER_BOUND('',#786,.T.);
#472=FACE_OUTER_BOUND('',#787,.T.);
#473=FACE_OUTER_BOUND('',#788,.T.);
#474=FACE_OUTER_BOUND('',#789,.T.);
#475=FACE_OUTER_BOUND('',#790,.T.);
#476=FACE_OUTER_BOUND('',#791,.T.);
#477=FACE_OUTER_BOUND('',#792,.T.);
#478=FACE_OUTER_BOUND('',#793,.T.);
#479=FACE_OUTER_BOUND('',#794,.T.);
#480=FACE_OUTER_BOUND('',#795,.T.);
#481=FACE_OUTER_BOUND('',#796,.T.);
#482=FACE_OUTER_BOUND('',#797,.T.);
#483=FACE_OUTER_BOUND('',#798,.T.);
#484=FACE_OUTER_BOUND('',#799,.T.);
#485=FACE_OUTER_BOUND('',#800,.T.);
#486=FACE_OUTER_BOUND('',#801,.T.);
#487=FACE_OUTER_BOUND('',#802,.T.);
#488=FACE_OUTER_BOUND('',#803,.T.);
#489=FACE_OUTER_BOUND('',#804,.T.);
#490=FACE_OUTER_BOUND('',#805,.T.);
#491=FACE_OUTER_BOUND('',#806,.T.);
#492=FACE_OUTER_BOUND('',#807,.T.);
#493=FACE_OUTER_BOUND('',#808,.T.);
#494=FACE_OUTER_BOUND('',#809,.T.);
#495=FACE_OUTER_BOUND('',#810,.T.);
#496=FACE_OUTER_BOUND('',#811,.T.);
#497=FACE_OUTER_BOUND('',#812,.T.);
#498=FACE_OUTER_BOUND('',#813,.T.);
#499=FACE_OUTER_BOUND('',#814,.T.);
#500=FACE_OUTER_BOUND('',#815,.T.);
#501=FACE_OUTER_BOUND('',#816,.T.);
#502=FACE_OUTER_BOUND('',#817,.T.);
#503=FACE_OUTER_BOUND('',#818,.T.);
#504=FACE_OUTER_BOUND('',#821,.T.);
#505=FACE_OUTER_BOUND('',#822,.T.);
#506=FACE_OUTER_BOUND('',#823,.T.);
#507=FACE_OUTER_BOUND('',#824,.T.);
#508=FACE_OUTER_BOUND('',#825,.T.);
#509=FACE_OUTER_BOUND('',#828,.T.);
#510=FACE_OUTER_BOUND('',#829,.T.);
#511=FACE_OUTER_BOUND('',#830,.T.);
#512=FACE_OUTER_BOUND('',#831,.T.);
#513=FACE_OUTER_BOUND('',#832,.T.);
#514=FACE_OUTER_BOUND('',#833,.T.);
#515=FACE_OUTER_BOUND('',#834,.T.);
#516=FACE_OUTER_BOUND('',#835,.T.);
#517=FACE_OUTER_BOUND('',#836,.T.);
#518=FACE_OUTER_BOUND('',#837,.T.);
#519=FACE_OUTER_BOUND('',#838,.T.);
#520=FACE_OUTER_BOUND('',#839,.T.);
#521=FACE_OUTER_BOUND('',#840,.T.);
#522=FACE_OUTER_BOUND('',#841,.T.);
#523=FACE_OUTER_BOUND('',#842,.T.);
#524=FACE_OUTER_BOUND('',#843,.T.);
#525=FACE_OUTER_BOUND('',#844,.T.);
#526=FACE_OUTER_BOUND('',#845,.T.);
#527=FACE_OUTER_BOUND('',#846,.T.);
#528=FACE_OUTER_BOUND('',#848,.T.);
#529=FACE_OUTER_BOUND('',#849,.T.);
#530=FACE_OUTER_BOUND('',#851,.T.);
#531=FACE_OUTER_BOUND('',#852,.T.);
#532=FACE_OUTER_BOUND('',#853,.T.);
#533=FACE_OUTER_BOUND('',#855,.T.);
#534=FACE_OUTER_BOUND('',#856,.T.);
#535=FACE_OUTER_BOUND('',#857,.T.);
#536=FACE_OUTER_BOUND('',#858,.T.);
#537=FACE_OUTER_BOUND('',#859,.T.);
#538=FACE_OUTER_BOUND('',#861,.T.);
#539=FACE_OUTER_BOUND('',#862,.T.);
#540=FACE_OUTER_BOUND('',#863,.T.);
#541=FACE_OUTER_BOUND('',#864,.T.);
#542=FACE_OUTER_BOUND('',#866,.T.);
#543=FACE_OUTER_BOUND('',#867,.T.);
#544=FACE_OUTER_BOUND('',#869,.T.);
#545=FACE_OUTER_BOUND('',#870,.T.);
#546=FACE_OUTER_BOUND('',#871,.T.);
#547=FACE_OUTER_BOUND('',#872,.T.);
#548=FACE_OUTER_BOUND('',#873,.T.);
#549=FACE_OUTER_BOUND('',#874,.T.);
#550=FACE_OUTER_BOUND('',#876,.T.);
#551=FACE_OUTER_BOUND('',#877,.T.);
#552=FACE_OUTER_BOUND('',#879,.T.);
#553=FACE_OUTER_BOUND('',#881,.T.);
#554=FACE_OUTER_BOUND('',#882,.T.);
#555=FACE_OUTER_BOUND('',#884,.T.);
#556=FACE_OUTER_BOUND('',#885,.T.);
#557=FACE_OUTER_BOUND('',#887,.T.);
#558=FACE_OUTER_BOUND('',#888,.T.);
#559=FACE_OUTER_BOUND('',#890,.T.);
#560=FACE_OUTER_BOUND('',#892,.T.);
#561=FACE_OUTER_BOUND('',#893,.T.);
#562=FACE_OUTER_BOUND('',#895,.T.);
#563=FACE_OUTER_BOUND('',#896,.T.);
#564=FACE_OUTER_BOUND('',#897,.T.);
#565=FACE_OUTER_BOUND('',#899,.T.);
#566=FACE_OUTER_BOUND('',#900,.T.);
#567=FACE_OUTER_BOUND('',#902,.T.);
#568=FACE_OUTER_BOUND('',#903,.T.);
#569=FACE_OUTER_BOUND('',#905,.T.);
#570=FACE_OUTER_BOUND('',#906,.T.);
#571=FACE_OUTER_BOUND('',#908,.T.);
#572=FACE_OUTER_BOUND('',#909,.T.);
#573=FACE_OUTER_BOUND('',#911,.T.);
#574=FACE_OUTER_BOUND('',#912,.T.);
#575=FACE_OUTER_BOUND('',#913,.T.);
#576=FACE_OUTER_BOUND('',#915,.T.);
#577=EDGE_LOOP('',(#3275,#3276,#3277,#3278,#3279,#3280,#3281,#3282,#3283,
#3284,#3285,#3286,#3287,#3288));
#578=EDGE_LOOP('',(#3289,#3290,#3291,#3292));
#579=EDGE_LOOP('',(#3293,#3294,#3295,#3296));
#580=EDGE_LOOP('',(#3297,#3298,#3299,#3300));
#581=EDGE_LOOP('',(#3301));
#582=EDGE_LOOP('',(#3302));
#583=EDGE_LOOP('',(#3303,#3304,#3305,#3306));
#584=EDGE_LOOP('',(#3307,#3308,#3309,#3310));
#585=EDGE_LOOP('',(#3311,#3312,#3313,#3314));
#586=EDGE_LOOP('',(#3315,#3316,#3317,#3318));
#587=EDGE_LOOP('',(#3319,#3320,#3321,#3322,#3323,#3324,#3325,#3326,#3327,
#3328,#3329,#3330,#3331,#3332));
#588=EDGE_LOOP('',(#3333));
#589=EDGE_LOOP('',(#3334));
#590=EDGE_LOOP('',(#3335));
#591=EDGE_LOOP('',(#3336));
#592=EDGE_LOOP('',(#3337,#3338,#3339,#3340));
#593=EDGE_LOOP('',(#3341,#3342,#3343,#3344));
#594=EDGE_LOOP('',(#3345,#3346,#3347,#3348));
#595=EDGE_LOOP('',(#3349,#3350,#3351,#3352));
#596=EDGE_LOOP('',(#3353,#3354,#3355,#3356,#3357,#3358,#3359,#3360,#3361));
#597=EDGE_LOOP('',(#3362,#3363,#3364,#3365,#3366,#3367));
#598=EDGE_LOOP('',(#3368,#3369,#3370,#3371,#3372,#3373));
#599=EDGE_LOOP('',(#3374,#3375,#3376,#3377,#3378,#3379));
#600=EDGE_LOOP('',(#3380,#3381,#3382,#3383));
#601=EDGE_LOOP('',(#3384,#3385,#3386,#3387,#3388,#3389,#3390));
#602=EDGE_LOOP('',(#3391,#3392,#3393,#3394));
#603=EDGE_LOOP('',(#3395,#3396,#3397,#3398));
#604=EDGE_LOOP('',(#3399,#3400,#3401,#3402));
#605=EDGE_LOOP('',(#3403,#3404,#3405,#3406));
#606=EDGE_LOOP('',(#3407,#3408,#3409,#3410,#3411,#3412,#3413,#3414));
#607=EDGE_LOOP('',(#3415,#3416,#3417,#3418,#3419,#3420,#3421,#3422));
#608=EDGE_LOOP('',(#3423,#3424,#3425,#3426,#3427,#3428,#3429,#3430));
#609=EDGE_LOOP('',(#3431,#3432,#3433,#3434));
#610=EDGE_LOOP('',(#3435,#3436,#3437,#3438));
#611=EDGE_LOOP('',(#3439,#3440,#3441,#3442));
#612=EDGE_LOOP('',(#3443,#3444,#3445,#3446));
#613=EDGE_LOOP('',(#3447,#3448,#3449,#3450));
#614=EDGE_LOOP('',(#3451,#3452,#3453,#3454));
#615=EDGE_LOOP('',(#3455,#3456,#3457,#3458));
#616=EDGE_LOOP('',(#3459,#3460,#3461,#3462));
#617=EDGE_LOOP('',(#3463,#3464,#3465,#3466));
#618=EDGE_LOOP('',(#3467,#3468,#3469,#3470));
#619=EDGE_LOOP('',(#3471,#3472,#3473,#3474));
#620=EDGE_LOOP('',(#3475,#3476,#3477,#3478));
#621=EDGE_LOOP('',(#3479,#3480,#3481));
#622=EDGE_LOOP('',(#3482,#3483,#3484));
#623=EDGE_LOOP('',(#3485,#3486,#3487));
#624=EDGE_LOOP('',(#3488,#3489,#3490));
#625=EDGE_LOOP('',(#3491,#3492,#3493));
#626=EDGE_LOOP('',(#3494,#3495,#3496));
#627=EDGE_LOOP('',(#3497,#3498,#3499,#3500));
#628=EDGE_LOOP('',(#3501,#3502,#3503));
#629=EDGE_LOOP('',(#3504,#3505,#3506));
#630=EDGE_LOOP('',(#3507,#3508,#3509));
#631=EDGE_LOOP('',(#3510,#3511,#3512,#3513,#3514,#3515,#3516,#3517,#3518,
#3519,#3520,#3521,#3522,#3523,#3524,#3525,#3526,#3527,#3528,#3529));
#632=EDGE_LOOP('',(#3530,#3531,#3532,#3533));
#633=EDGE_LOOP('',(#3534,#3535,#3536,#3537));
#634=EDGE_LOOP('',(#3538,#3539,#3540,#3541));
#635=EDGE_LOOP('',(#3542,#3543,#3544,#3545));
#636=EDGE_LOOP('',(#3546,#3547,#3548,#3549));
#637=EDGE_LOOP('',(#3550,#3551,#3552,#3553));
#638=EDGE_LOOP('',(#3554,#3555,#3556,#3557));
#639=EDGE_LOOP('',(#3558,#3559,#3560,#3561));
#640=EDGE_LOOP('',(#3562,#3563,#3564,#3565));
#641=EDGE_LOOP('',(#3566,#3567,#3568,#3569));
#642=EDGE_LOOP('',(#3570,#3571,#3572));
#643=EDGE_LOOP('',(#3573,#3574,#3575));
#644=EDGE_LOOP('',(#3576,#3577,#3578));
#645=EDGE_LOOP('',(#3579,#3580,#3581,#3582));
#646=EDGE_LOOP('',(#3583,#3584,#3585,#3586));
#647=EDGE_LOOP('',(#3587,#3588,#3589,#3590));
#648=EDGE_LOOP('',(#3591,#3592,#3593));
#649=EDGE_LOOP('',(#3594,#3595,#3596));
#650=EDGE_LOOP('',(#3597,#3598,#3599,#3600));
#651=EDGE_LOOP('',(#3601,#3602,#3603,#3604));
#652=EDGE_LOOP('',(#3605,#3606,#3607,#3608));
#653=EDGE_LOOP('',(#3609,#3610,#3611,#3612));
#654=EDGE_LOOP('',(#3613,#3614,#3615,#3616,#3617,#3618,#3619,#3620,#3621,
#3622,#3623,#3624,#3625,#3626,#3627,#3628,#3629,#3630,#3631,#3632));
#655=EDGE_LOOP('',(#3633,#3634,#3635,#3636));
#656=EDGE_LOOP('',(#3637,#3638,#3639,#3640,#3641,#3642,#3643,#3644));
#657=EDGE_LOOP('',(#3645,#3646,#3647,#3648,#3649,#3650,#3651,#3652,#3653,
#3654,#3655,#3656,#3657,#3658,#3659,#3660,#3661,#3662,#3663));
#658=EDGE_LOOP('',(#3664,#3665,#3666,#3667));
#659=EDGE_LOOP('',(#3668));
#660=EDGE_LOOP('',(#3669));
#661=EDGE_LOOP('',(#3670));
#662=EDGE_LOOP('',(#3671));
#663=EDGE_LOOP('',(#3672));
#664=EDGE_LOOP('',(#3673,#3674,#3675,#3676,#3677,#3678,#3679,#3680,#3681,
#3682,#3683,#3684,#3685,#3686,#3687,#3688,#3689,#3690,#3691));
#665=EDGE_LOOP('',(#3692,#3693,#3694,#3695));
#666=EDGE_LOOP('',(#3696));
#667=EDGE_LOOP('',(#3697));
#668=EDGE_LOOP('',(#3698));
#669=EDGE_LOOP('',(#3699));
#670=EDGE_LOOP('',(#3700));
#671=EDGE_LOOP('',(#3701,#3702,#3703,#3704));
#672=EDGE_LOOP('',(#3705,#3706,#3707,#3708));
#673=EDGE_LOOP('',(#3709,#3710,#3711,#3712));
#674=EDGE_LOOP('',(#3713,#3714,#3715,#3716));
#675=EDGE_LOOP('',(#3717,#3718,#3719,#3720));
#676=EDGE_LOOP('',(#3721,#3722,#3723,#3724));
#677=EDGE_LOOP('',(#3725,#3726,#3727,#3728));
#678=EDGE_LOOP('',(#3729,#3730,#3731,#3732));
#679=EDGE_LOOP('',(#3733,#3734,#3735,#3736));
#680=EDGE_LOOP('',(#3737,#3738,#3739));
#681=EDGE_LOOP('',(#3740,#3741,#3742));
#682=EDGE_LOOP('',(#3743,#3744,#3745));
#683=EDGE_LOOP('',(#3746,#3747,#3748));
#684=EDGE_LOOP('',(#3749,#3750,#3751));
#685=EDGE_LOOP('',(#3752,#3753,#3754));
#686=EDGE_LOOP('',(#3755,#3756,#3757,#3758));
#687=EDGE_LOOP('',(#3759,#3760,#3761));
#688=EDGE_LOOP('',(#3762,#3763,#3764));
#689=EDGE_LOOP('',(#3765,#3766,#3767));
#690=EDGE_LOOP('',(#3768,#3769,#3770));
#691=EDGE_LOOP('',(#3771,#3772,#3773));
#692=EDGE_LOOP('',(#3774,#3775,#3776,#3777,#3778,#3779,#3780,#3781,#3782,
#3783,#3784,#3785,#3786,#3787,#3788,#3789,#3790,#3791,#3792,#3793));
#693=EDGE_LOOP('',(#3794,#3795,#3796,#3797,#3798,#3799,#3800,#3801,#3802,
#3803,#3804,#3805,#3806,#3807,#3808,#3809,#3810,#3811,#3812,#3813,#3814,
#3815,#3816,#3817,#3818,#3819,#3820,#3821,#3822,#3823,#3824,#3825,#3826,
#3827,#3828,#3829));
#694=EDGE_LOOP('',(#3830,#3831,#3832,#3833));
#695=EDGE_LOOP('',(#3834,#3835,#3836,#3837));
#696=EDGE_LOOP('',(#3838,#3839,#3840,#3841));
#697=EDGE_LOOP('',(#3842,#3843,#3844,#3845));
#698=EDGE_LOOP('',(#3846,#3847,#3848,#3849));
#699=EDGE_LOOP('',(#3850,#3851,#3852,#3853));
#700=EDGE_LOOP('',(#3854,#3855,#3856,#3857));
#701=EDGE_LOOP('',(#3858,#3859,#3860,#3861));
#702=EDGE_LOOP('',(#3862,#3863,#3864,#3865,#3866));
#703=EDGE_LOOP('',(#3867,#3868,#3869,#3870));
#704=EDGE_LOOP('',(#3871,#3872,#3873,#3874,#3875));
#705=EDGE_LOOP('',(#3876,#3877,#3878,#3879));
#706=EDGE_LOOP('',(#3880,#3881,#3882,#3883,#3884));
#707=EDGE_LOOP('',(#3885,#3886,#3887,#3888,#3889));
#708=EDGE_LOOP('',(#3890,#3891,#3892,#3893,#3894));
#709=EDGE_LOOP('',(#3895,#3896,#3897,#3898));
#710=EDGE_LOOP('',(#3899,#3900,#3901,#3902,#3903));
#711=EDGE_LOOP('',(#3904,#3905,#3906,#3907,#3908));
#712=EDGE_LOOP('',(#3909,#3910,#3911,#3912));
#713=EDGE_LOOP('',(#3913,#3914,#3915,#3916,#3917));
#714=EDGE_LOOP('',(#3918,#3919,#3920,#3921,#3922));
#715=EDGE_LOOP('',(#3923,#3924,#3925,#3926));
#716=EDGE_LOOP('',(#3927,#3928,#3929,#3930,#3931));
#717=EDGE_LOOP('',(#3932,#3933,#3934,#3935,#3936));
#718=EDGE_LOOP('',(#3937,#3938,#3939,#3940));
#719=EDGE_LOOP('',(#3941,#3942,#3943,#3944,#3945));
#720=EDGE_LOOP('',(#3946,#3947,#3948,#3949));
#721=EDGE_LOOP('',(#3950,#3951,#3952,#3953,#3954));
#722=EDGE_LOOP('',(#3955,#3956,#3957,#3958,#3959));
#723=EDGE_LOOP('',(#3960,#3961,#3962,#3963));
#724=EDGE_LOOP('',(#3964,#3965,#3966,#3967,#3968));
#725=EDGE_LOOP('',(#3969,#3970,#3971,#3972,#3973));
#726=EDGE_LOOP('',(#3974,#3975,#3976,#3977));
#727=EDGE_LOOP('',(#3978,#3979,#3980,#3981));
#728=EDGE_LOOP('',(#3982,#3983,#3984,#3985));
#729=EDGE_LOOP('',(#3986,#3987,#3988,#3989));
#730=EDGE_LOOP('',(#3990,#3991,#3992,#3993));
#731=EDGE_LOOP('',(#3994,#3995,#3996,#3997));
#732=EDGE_LOOP('',(#3998,#3999,#4000,#4001));
#733=EDGE_LOOP('',(#4002,#4003,#4004,#4005));
#734=EDGE_LOOP('',(#4006,#4007,#4008,#4009));
#735=EDGE_LOOP('',(#4010,#4011,#4012,#4013));
#736=EDGE_LOOP('',(#4014,#4015,#4016,#4017));
#737=EDGE_LOOP('',(#4018,#4019,#4020,#4021));
#738=EDGE_LOOP('',(#4022,#4023,#4024,#4025));
#739=EDGE_LOOP('',(#4026,#4027,#4028,#4029));
#740=EDGE_LOOP('',(#4030,#4031,#4032,#4033));
#741=EDGE_LOOP('',(#4034,#4035,#4036,#4037));
#742=EDGE_LOOP('',(#4038,#4039,#4040));
#743=EDGE_LOOP('',(#4041,#4042,#4043,#4044));
#744=EDGE_LOOP('',(#4045,#4046,#4047));
#745=EDGE_LOOP('',(#4048,#4049,#4050,#4051));
#746=EDGE_LOOP('',(#4052,#4053,#4054));
#747=EDGE_LOOP('',(#4055,#4056,#4057));
#748=EDGE_LOOP('',(#4058,#4059,#4060));
#749=EDGE_LOOP('',(#4061,#4062,#4063,#4064));
#750=EDGE_LOOP('',(#4065,#4066,#4067));
#751=EDGE_LOOP('',(#4068,#4069,#4070,#4071));
#752=EDGE_LOOP('',(#4072,#4073,#4074));
#753=EDGE_LOOP('',(#4075,#4076,#4077,#4078));
#754=EDGE_LOOP('',(#4079,#4080,#4081,#4082));
#755=EDGE_LOOP('',(#4083,#4084,#4085,#4086));
#756=EDGE_LOOP('',(#4087,#4088,#4089,#4090,#4091,#4092,#4093,#4094,#4095,
#4096,#4097,#4098,#4099,#4100,#4101,#4102,#4103,#4104,#4105,#4106));
#757=EDGE_LOOP('',(#4107,#4108,#4109,#4110,#4111,#4112,#4113,#4114,#4115,
#4116,#4117,#4118,#4119,#4120,#4121,#4122,#4123,#4124,#4125,#4126,#4127,
#4128,#4129,#4130,#4131,#4132,#4133,#4134,#4135,#4136,#4137,#4138,#4139,
#4140,#4141,#4142));
#758=EDGE_LOOP('',(#4143,#4144,#4145,#4146));
#759=EDGE_LOOP('',(#4147,#4148,#4149,#4150));
#760=EDGE_LOOP('',(#4151,#4152,#4153,#4154));
#761=EDGE_LOOP('',(#4155,#4156,#4157,#4158));
#762=EDGE_LOOP('',(#4159,#4160,#4161,#4162));
#763=EDGE_LOOP('',(#4163,#4164,#4165,#4166));
#764=EDGE_LOOP('',(#4167,#4168,#4169,#4170));
#765=EDGE_LOOP('',(#4171,#4172,#4173,#4174));
#766=EDGE_LOOP('',(#4175,#4176,#4177,#4178));
#767=EDGE_LOOP('',(#4179,#4180,#4181,#4182,#4183,#4184));
#768=EDGE_LOOP('',(#4185,#4186,#4187,#4188));
#769=EDGE_LOOP('',(#4189,#4190,#4191,#4192,#4193,#4194));
#770=EDGE_LOOP('',(#4195,#4196,#4197,#4198));
#771=EDGE_LOOP('',(#4199,#4200,#4201,#4202,#4203,#4204));
#772=EDGE_LOOP('',(#4205,#4206,#4207,#4208));
#773=EDGE_LOOP('',(#4209,#4210,#4211,#4212,#4213,#4214));
#774=EDGE_LOOP('',(#4215,#4216,#4217,#4218));
#775=EDGE_LOOP('',(#4219,#4220,#4221,#4222,#4223,#4224));
#776=EDGE_LOOP('',(#4225,#4226,#4227,#4228));
#777=EDGE_LOOP('',(#4229,#4230,#4231,#4232,#4233,#4234));
#778=EDGE_LOOP('',(#4235,#4236,#4237,#4238));
#779=EDGE_LOOP('',(#4239,#4240,#4241,#4242,#4243,#4244));
#780=EDGE_LOOP('',(#4245,#4246,#4247,#4248));
#781=EDGE_LOOP('',(#4249,#4250,#4251,#4252,#4253,#4254));
#782=EDGE_LOOP('',(#4255,#4256,#4257,#4258));
#783=EDGE_LOOP('',(#4259,#4260,#4261,#4262,#4263,#4264));
#784=EDGE_LOOP('',(#4265,#4266,#4267,#4268));
#785=EDGE_LOOP('',(#4269,#4270,#4271,#4272,#4273,#4274));
#786=EDGE_LOOP('',(#4275,#4276,#4277,#4278));
#787=EDGE_LOOP('',(#4279,#4280,#4281,#4282,#4283,#4284));
#788=EDGE_LOOP('',(#4285,#4286,#4287,#4288));
#789=EDGE_LOOP('',(#4289,#4290,#4291,#4292,#4293,#4294));
#790=EDGE_LOOP('',(#4295,#4296,#4297,#4298));
#791=EDGE_LOOP('',(#4299,#4300,#4301,#4302,#4303,#4304));
#792=EDGE_LOOP('',(#4305,#4306,#4307,#4308));
#793=EDGE_LOOP('',(#4309,#4310,#4311,#4312,#4313,#4314));
#794=EDGE_LOOP('',(#4315,#4316,#4317,#4318));
#795=EDGE_LOOP('',(#4319,#4320,#4321,#4322,#4323,#4324));
#796=EDGE_LOOP('',(#4325,#4326,#4327,#4328));
#797=EDGE_LOOP('',(#4329,#4330,#4331,#4332,#4333,#4334));
#798=EDGE_LOOP('',(#4335,#4336,#4337,#4338));
#799=EDGE_LOOP('',(#4339,#4340,#4341,#4342));
#800=EDGE_LOOP('',(#4343,#4344,#4345,#4346));
#801=EDGE_LOOP('',(#4347,#4348,#4349,#4350));
#802=EDGE_LOOP('',(#4351,#4352,#4353,#4354));
#803=EDGE_LOOP('',(#4355,#4356,#4357,#4358));
#804=EDGE_LOOP('',(#4359,#4360,#4361,#4362));
#805=EDGE_LOOP('',(#4363,#4364,#4365,#4366));
#806=EDGE_LOOP('',(#4367,#4368,#4369,#4370));
#807=EDGE_LOOP('',(#4371,#4372,#4373,#4374));
#808=EDGE_LOOP('',(#4375,#4376,#4377,#4378));
#809=EDGE_LOOP('',(#4379,#4380,#4381,#4382));
#810=EDGE_LOOP('',(#4383,#4384,#4385,#4386));
#811=EDGE_LOOP('',(#4387,#4388,#4389,#4390));
#812=EDGE_LOOP('',(#4391,#4392,#4393,#4394));
#813=EDGE_LOOP('',(#4395,#4396,#4397,#4398));
#814=EDGE_LOOP('',(#4399,#4400,#4401,#4402));
#815=EDGE_LOOP('',(#4403,#4404,#4405,#4406,#4407,#4408,#4409,#4410,#4411,
#4412,#4413,#4414,#4415,#4416));
#816=EDGE_LOOP('',(#4417,#4418,#4419,#4420));
#817=EDGE_LOOP('',(#4421,#4422,#4423,#4424));
#818=EDGE_LOOP('',(#4425,#4426,#4427,#4428));
#819=EDGE_LOOP('',(#4429));
#820=EDGE_LOOP('',(#4430));
#821=EDGE_LOOP('',(#4431,#4432,#4433,#4434));
#822=EDGE_LOOP('',(#4435,#4436,#4437,#4438));
#823=EDGE_LOOP('',(#4439,#4440,#4441,#4442));
#824=EDGE_LOOP('',(#4443,#4444,#4445,#4446));
#825=EDGE_LOOP('',(#4447,#4448,#4449,#4450,#4451,#4452,#4453,#4454,#4455,
#4456,#4457,#4458,#4459,#4460));
#826=EDGE_LOOP('',(#4461));
#827=EDGE_LOOP('',(#4462));
#828=EDGE_LOOP('',(#4463));
#829=EDGE_LOOP('',(#4464));
#830=EDGE_LOOP('',(#4465,#4466,#4467,#4468));
#831=EDGE_LOOP('',(#4469,#4470,#4471,#4472));
#832=EDGE_LOOP('',(#4473,#4474,#4475,#4476));
#833=EDGE_LOOP('',(#4477,#4478,#4479,#4480));
#834=EDGE_LOOP('',(#4481,#4482,#4483,#4484,#4485,#4486,#4487,#4488,#4489));
#835=EDGE_LOOP('',(#4490,#4491,#4492,#4493,#4494,#4495));
#836=EDGE_LOOP('',(#4496,#4497,#4498,#4499,#4500,#4501));
#837=EDGE_LOOP('',(#4502,#4503,#4504,#4505,#4506,#4507));
#838=EDGE_LOOP('',(#4508,#4509,#4510,#4511));
#839=EDGE_LOOP('',(#4512,#4513,#4514,#4515,#4516,#4517,#4518));
#840=EDGE_LOOP('',(#4519,#4520,#4521,#4522));
#841=EDGE_LOOP('',(#4523,#4524,#4525,#4526,#4527,#4528));
#842=EDGE_LOOP('',(#4529));
#843=EDGE_LOOP('',(#4530));
#844=EDGE_LOOP('',(#4531,#4532,#4533,#4534,#4535));
#845=EDGE_LOOP('',(#4536,#4537,#4538,#4539,#4540));
#846=EDGE_LOOP('',(#4541));
#847=EDGE_LOOP('',(#4542));
#848=EDGE_LOOP('',(#4543,#4544,#4545,#4546));
#849=EDGE_LOOP('',(#4547));
#850=EDGE_LOOP('',(#4548));
#851=EDGE_LOOP('',(#4549,#4550,#4551,#4552));
#852=EDGE_LOOP('',(#4553,#4554,#4555,#4556,#4557));
#853=EDGE_LOOP('',(#4558));
#854=EDGE_LOOP('',(#4559));
#855=EDGE_LOOP('',(#4560,#4561,#4562,#4563,#4564));
#856=EDGE_LOOP('',(#4565,#4566,#4567,#4568,#4569));
#857=EDGE_LOOP('',(#4570,#4571,#4572,#4573,#4574));
#858=EDGE_LOOP('',(#4575,#4576,#4577,#4578,#4579));
#859=EDGE_LOOP('',(#4580));
#860=EDGE_LOOP('',(#4581));
#861=EDGE_LOOP('',(#4582,#4583,#4584,#4585,#4586));
#862=EDGE_LOOP('',(#4587,#4588,#4589,#4590,#4591));
#863=EDGE_LOOP('',(#4592,#4593,#4594,#4595,#4596));
#864=EDGE_LOOP('',(#4597));
#865=EDGE_LOOP('',(#4598));
#866=EDGE_LOOP('',(#4599,#4600,#4601,#4602));
#867=EDGE_LOOP('',(#4603));
#868=EDGE_LOOP('',(#4604));
#869=EDGE_LOOP('',(#4605,#4606,#4607,#4608));
#870=EDGE_LOOP('',(#4609,#4610,#4611,#4612));
#871=EDGE_LOOP('',(#4613,#4614,#4615,#4616));
#872=EDGE_LOOP('',(#4617,#4618,#4619,#4620));
#873=EDGE_LOOP('',(#4621,#4622,#4623,#4624));
#874=EDGE_LOOP('',(#4625));
#875=EDGE_LOOP('',(#4626));
#876=EDGE_LOOP('',(#4627,#4628,#4629,#4630));
#877=EDGE_LOOP('',(#4631));
#878=EDGE_LOOP('',(#4632));
#879=EDGE_LOOP('',(#4633));
#880=EDGE_LOOP('',(#4634));
#881=EDGE_LOOP('',(#4635,#4636,#4637,#4638));
#882=EDGE_LOOP('',(#4639));
#883=EDGE_LOOP('',(#4640));
#884=EDGE_LOOP('',(#4641,#4642,#4643,#4644));
#885=EDGE_LOOP('',(#4645));
#886=EDGE_LOOP('',(#4646));
#887=EDGE_LOOP('',(#4647,#4648,#4649,#4650));
#888=EDGE_LOOP('',(#4651));
#889=EDGE_LOOP('',(#4652));
#890=EDGE_LOOP('',(#4653));
#891=EDGE_LOOP('',(#4654));
#892=EDGE_LOOP('',(#4655,#4656,#4657,#4658));
#893=EDGE_LOOP('',(#4659));
#894=EDGE_LOOP('',(#4660));
#895=EDGE_LOOP('',(#4661,#4662,#4663,#4664));
#896=EDGE_LOOP('',(#4665,#4666,#4667,#4668));
#897=EDGE_LOOP('',(#4669));
#898=EDGE_LOOP('',(#4670));
#899=EDGE_LOOP('',(#4671,#4672,#4673,#4674));
#900=EDGE_LOOP('',(#4675));
#901=EDGE_LOOP('',(#4676));
#902=EDGE_LOOP('',(#4677,#4678,#4679,#4680));
#903=EDGE_LOOP('',(#4681));
#904=EDGE_LOOP('',(#4682));
#905=EDGE_LOOP('',(#4683,#4684,#4685,#4686));
#906=EDGE_LOOP('',(#4687));
#907=EDGE_LOOP('',(#4688));
#908=EDGE_LOOP('',(#4689,#4690,#4691,#4692));
#909=EDGE_LOOP('',(#4693));
#910=EDGE_LOOP('',(#4694));
#911=EDGE_LOOP('',(#4695,#4696,#4697,#4698));
#912=EDGE_LOOP('',(#4699,#4700,#4701,#4702));
#913=EDGE_LOOP('',(#4703));
#914=EDGE_LOOP('',(#4704));
#915=EDGE_LOOP('',(#4705,#4706,#4707,#4708));
#916=CIRCLE('',#5262,0.00499999999999998);
#917=CIRCLE('',#5263,0.005);
#918=CIRCLE('',#5264,0.005);
#919=CIRCLE('',#5265,0.005);
#920=CIRCLE('',#5266,0.00500000000000002);
#921=CIRCLE('',#5267,0.00499999999999998);
#922=CIRCLE('',#5268,0.00500000000000002);
#923=CIRCLE('',#5269,0.00500000000000002);
#924=CIRCLE('',#5273,0.007625);
#925=CIRCLE('',#5274,0.007625);
#926=CIRCLE('',#5277,0.004225);
#927=CIRCLE('',#5278,0.004225);
#928=CIRCLE('',#5281,0.004225);
#929=CIRCLE('',#5282,0.004225);
#930=CIRCLE('',#5284,0.005);
#931=CIRCLE('',#5285,0.005);
#932=CIRCLE('',#5286,0.005);
#933=CIRCLE('',#5287,0.005);
#934=CIRCLE('',#5288,0.005);
#935=CIRCLE('',#5289,0.005);
#936=CIRCLE('',#5290,0.005);
#937=CIRCLE('',#5291,0.005);
#938=CIRCLE('',#5299,0.007625);
#939=CIRCLE('',#5300,0.007625);
#940=CIRCLE('',#5301,0.007625);
#941=CIRCLE('',#5320,0.0076);
#942=CIRCLE('',#5322,0.0076);
#943=CIRCLE('',#5324,0.0076);
#944=CIRCLE('',#5326,0.0076);
#945=CIRCLE('',#5328,0.0076);
#946=CIRCLE('',#5330,0.0076);
#947=CIRCLE('',#5333,0.0076);
#948=CIRCLE('',#5335,0.0076);
#949=CIRCLE('',#5337,0.0076);
#950=CIRCLE('',#5342,0.0076);
#951=CIRCLE('',#5344,0.0076);
#952=CIRCLE('',#5346,0.0076);
#953=CIRCLE('',#5351,0.0076);
#954=CIRCLE('',#5353,0.0076);
#955=CIRCLE('',#5362,0.0076);
#956=CIRCLE('',#5363,0.005);
#957=CIRCLE('',#5364,0.0076);
#958=CIRCLE('',#5366,0.00123);
#959=CIRCLE('',#5367,0.00123);
#960=CIRCLE('',#5368,0.00123);
#961=CIRCLE('',#5369,0.00123);
#962=CIRCLE('',#5370,0.0125);
#963=CIRCLE('',#5372,0.0076);
#964=CIRCLE('',#5373,0.0076);
#965=CIRCLE('',#5374,0.005);
#966=CIRCLE('',#5376,0.00123);
#967=CIRCLE('',#5377,0.00123);
#968=CIRCLE('',#5378,0.00123);
#969=CIRCLE('',#5379,0.00123);
#970=CIRCLE('',#5380,0.0125);
#971=CIRCLE('',#5391,0.0076);
#972=CIRCLE('',#5393,0.0076);
#973=CIRCLE('',#5395,0.0076);
#974=CIRCLE('',#5397,0.0076);
#975=CIRCLE('',#5399,0.0076);
#976=CIRCLE('',#5401,0.0076);
#977=CIRCLE('',#5404,0.0076);
#978=CIRCLE('',#5406,0.0076);
#979=CIRCLE('',#5408,0.0076);
#980=CIRCLE('',#5410,0.0076);
#981=CIRCLE('',#5412,0.0076);
#982=CIRCLE('',#5415,0.0076);
#983=CIRCLE('',#5416,0.0076);
#984=CIRCLE('',#5417,0.0076);
#985=CIRCLE('',#5418,0.0076);
#986=CIRCLE('',#5419,0.0076);
#987=CIRCLE('',#5420,0.0076);
#988=CIRCLE('',#5421,0.0076);
#989=CIRCLE('',#5422,0.0076);
#990=CIRCLE('',#5423,0.0076);
#991=CIRCLE('',#5424,0.0076);
#992=CIRCLE('',#5425,0.0076);
#993=CIRCLE('',#5426,0.0076);
#994=CIRCLE('',#5427,0.0076);
#995=CIRCLE('',#5428,0.0076);
#996=CIRCLE('',#5429,0.0076);
#997=CIRCLE('',#5430,0.0076);
#998=CIRCLE('',#5432,0.0023);
#999=CIRCLE('',#5433,0.0023);
#1000=CIRCLE('',#5436,0.0023);
#1001=CIRCLE('',#5437,0.0023);
#1002=CIRCLE('',#5440,0.0023);
#1003=CIRCLE('',#5441,0.0023);
#1004=CIRCLE('',#5443,0.0023);
#1005=CIRCLE('',#5444,0.0023);
#1006=CIRCLE('',#5446,0.0023);
#1007=CIRCLE('',#5447,0.0023);
#1008=CIRCLE('',#5450,0.0023);
#1009=CIRCLE('',#5451,0.0023);
#1010=CIRCLE('',#5453,0.0023);
#1011=CIRCLE('',#5454,0.0023);
#1012=CIRCLE('',#5457,0.0023);
#1013=CIRCLE('',#5458,0.0023);
#1014=CIRCLE('',#5460,0.0023);
#1015=CIRCLE('',#5461,0.0023);
#1016=CIRCLE('',#5464,0.0023);
#1017=CIRCLE('',#5465,0.0023);
#1018=CIRCLE('',#5467,0.0023);
#1019=CIRCLE('',#5468,0.0023);
#1020=CIRCLE('',#5471,0.0023);
#1021=CIRCLE('',#5472,0.0023);
#1022=CIRCLE('',#5475,0.0023);
#1023=CIRCLE('',#5476,0.0023);
#1024=CIRCLE('',#5478,0.0023);
#1025=CIRCLE('',#5479,0.0023);
#1026=CIRCLE('',#5482,0.0023);
#1027=CIRCLE('',#5483,0.0023);
#1028=CIRCLE('',#5485,0.0023);
#1029=CIRCLE('',#5486,0.0023);
#1030=CIRCLE('',#5504,0.0076);
#1031=CIRCLE('',#5507,0.0076);
#1032=CIRCLE('',#5510,0.0076);
#1033=CIRCLE('',#5512,0.0076);
#1034=CIRCLE('',#5514,0.0076);
#1035=CIRCLE('',#5517,0.0076);
#1036=CIRCLE('',#5520,0.0076);
#1037=CIRCLE('',#5526,0.0076);
#1038=CIRCLE('',#5527,0.0076);
#1039=CIRCLE('',#5528,0.0076);
#1040=CIRCLE('',#5529,0.0076);
#1041=CIRCLE('',#5530,0.0076);
#1042=CIRCLE('',#5531,0.0076);
#1043=CIRCLE('',#5532,0.0076);
#1044=CIRCLE('',#5533,0.0076);
#1045=CIRCLE('',#5534,0.0076);
#1046=CIRCLE('',#5535,0.0076);
#1047=CIRCLE('',#5536,0.0076);
#1048=CIRCLE('',#5537,0.0076);
#1049=CIRCLE('',#5538,0.0076);
#1050=CIRCLE('',#5539,0.0076);
#1051=CIRCLE('',#5540,0.0076);
#1052=CIRCLE('',#5541,0.0076);
#1053=CIRCLE('',#5544,0.0023);
#1054=CIRCLE('',#5545,0.0023);
#1055=CIRCLE('',#5548,0.0023);
#1056=CIRCLE('',#5549,0.0023);
#1057=CIRCLE('',#5552,0.0023);
#1058=CIRCLE('',#5553,0.0023);
#1059=CIRCLE('',#5556,0.0023);
#1060=CIRCLE('',#5557,0.0023);
#1061=CIRCLE('',#5560,0.0023);
#1062=CIRCLE('',#5561,0.0023);
#1063=CIRCLE('',#5564,0.0023);
#1064=CIRCLE('',#5565,0.0023);
#1065=CIRCLE('',#5568,0.0023);
#1066=CIRCLE('',#5569,0.0023);
#1067=CIRCLE('',#5572,0.0023);
#1068=CIRCLE('',#5573,0.0023);
#1069=CIRCLE('',#5576,0.0023);
#1070=CIRCLE('',#5577,0.0023);
#1071=CIRCLE('',#5580,0.0023);
#1072=CIRCLE('',#5581,0.0023);
#1073=CIRCLE('',#5584,0.0023);
#1074=CIRCLE('',#5585,0.0023);
#1075=CIRCLE('',#5588,0.0023);
#1076=CIRCLE('',#5589,0.0023);
#1077=CIRCLE('',#5592,0.0023);
#1078=CIRCLE('',#5593,0.0023);
#1079=CIRCLE('',#5596,0.0023);
#1080=CIRCLE('',#5597,0.0023);
#1081=CIRCLE('',#5600,0.0023);
#1082=CIRCLE('',#5601,0.0023);
#1083=CIRCLE('',#5604,0.0023);
#1084=CIRCLE('',#5605,0.0023);
#1085=CIRCLE('',#5625,0.00500000000000005);
#1086=CIRCLE('',#5626,0.00500000000000002);
#1087=CIRCLE('',#5627,0.005);
#1088=CIRCLE('',#5628,0.005);
#1089=CIRCLE('',#5629,0.005);
#1090=CIRCLE('',#5630,0.00500000000000004);
#1091=CIRCLE('',#5631,0.005);
#1092=CIRCLE('',#5632,0.00500000000000002);
#1093=CIRCLE('',#5636,0.007625);
#1094=CIRCLE('',#5637,0.007625);
#1095=CIRCLE('',#5640,0.004225);
#1096=CIRCLE('',#5641,0.004225);
#1097=CIRCLE('',#5644,0.004225);
#1098=CIRCLE('',#5645,0.004225);
#1099=CIRCLE('',#5647,0.005);
#1100=CIRCLE('',#5648,0.005);
#1101=CIRCLE('',#5649,0.005);
#1102=CIRCLE('',#5650,0.005);
#1103=CIRCLE('',#5651,0.005);
#1104=CIRCLE('',#5652,0.005);
#1105=CIRCLE('',#5653,0.005);
#1106=CIRCLE('',#5654,0.005);
#1107=CIRCLE('',#5662,0.007625);
#1108=CIRCLE('',#5663,0.007625);
#1109=CIRCLE('',#5664,0.007625);
#1110=CIRCLE('',#5673,0.004);
#1111=CIRCLE('',#5674,0.004);
#1112=CIRCLE('',#5675,0.004);
#1113=CIRCLE('',#5676,0.004);
#1114=CIRCLE('',#5678,0.0025);
#1115=CIRCLE('',#5680,0.0025);
#1116=CIRCLE('',#5682,0.0015);
#1117=CIRCLE('',#5684,0.0015);
#1118=CIRCLE('',#5688,0.00700000000001);
#1119=CIRCLE('',#5689,0.00430000000001);
#1120=CIRCLE('',#5691,0.00700000000001);
#1121=CIRCLE('',#5693,0.00430000000001);
#1122=CIRCLE('',#5697,0.00650000000001);
#1123=CIRCLE('',#5698,0.00670000000001);
#1124=CIRCLE('',#5699,0.00650000000001);
#1125=CIRCLE('',#5701,0.00730000000001);
#1126=CIRCLE('',#5703,0.00650000000001);
#1127=CIRCLE('',#5705,0.00750000000001);
#1128=CIRCLE('',#5706,0.00750000000001);
#1129=CIRCLE('',#5708,0.00750000000001);
#1130=CIRCLE('',#5710,0.00650000000001);
#1131=CIRCLE('',#5711,0.00670000000001);
#1132=CIRCLE('',#5712,0.00650000000001);
#1133=CIRCLE('',#5714,0.00730000000001);
#1134=CIRCLE('',#5716,0.00650000000001);
#1135=CIRCLE('',#5718,0.00750000000001);
#1136=CIRCLE('',#5719,0.00750000000001);
#1137=CIRCLE('',#5721,0.00750000000001);
#1138=CIRCLE('',#5723,0.00700000010431813);
#1139=CIRCLE('',#5725,0.00700000010431813);
#1140=CIRCLE('',#5727,0.00630000000001);
#1141=CIRCLE('',#5729,0.00630000000001);
#1142=CIRCLE('',#5731,0.00590000000001);
#1143=CIRCLE('',#5733,0.00590000000001);
#1144=CIRCLE('',#5735,0.00630000000001);
#1145=CIRCLE('',#5737,0.00630000000001);
#1146=CIRCLE('',#5739,0.00700000010431813);
#1147=CIRCLE('',#5741,0.00700000010431813);
#1148=CIRCLE('',#5744,0.00715000000001);
#1149=CIRCLE('',#5746,0.00715000000001);
#1150=CIRCLE('',#5748,0.00750000000001);
#1151=CIRCLE('',#5750,0.00750000000001);
#1152=CIRCLE('',#5752,0.00715000000001);
#1153=CIRCLE('',#5754,0.00715000000001);
#1154=CIRCLE('',#5758,0.00650000000001);
#1155=CIRCLE('',#5759,0.00479999989272164);
#1156=CIRCLE('',#5761,0.00650000000001);
#1157=CIRCLE('',#5763,0.00455000000001);
#1158=CIRCLE('',#5765,0.00405000000001);
#1159=CIRCLE('',#5767,0.00405000000001);
#1160=CIRCLE('',#5769,0.00449999989942716);
#1161=CIRCLE('',#5773,0.00700000000001);
#1162=CIRCLE('',#5774,0.00430000000001);
#1163=CIRCLE('',#5776,0.00700000000001);
#1164=CIRCLE('',#5778,0.00430000000001);
#1165=CIRCLE('',#5782,0.00650000000001);
#1166=CIRCLE('',#5783,0.00479999989272164);
#1167=CIRCLE('',#5785,0.00650000000001);
#1168=CIRCLE('',#5787,0.00455000000001);
#1169=CIRCLE('',#5789,0.00405000000001);
#1170=CIRCLE('',#5791,0.00405000000001);
#1171=CIRCLE('',#5793,0.00449999989942716);
#1172=LINE('',#7393,#1627);
#1173=LINE('',#7397,#1628);
#1174=LINE('',#7401,#1629);
#1175=LINE('',#7405,#1630);
#1176=LINE('',#7409,#1631);
#1177=LINE('',#7415,#1632);
#1178=LINE('',#7422,#1633);
#1179=LINE('',#7423,#1634);
#1180=LINE('',#7424,#1635);
#1181=LINE('',#7427,#1636);
#1182=LINE('',#7429,#1637);
#1183=LINE('',#7430,#1638);
#1184=LINE('',#7433,#1639);
#1185=LINE('',#7435,#1640);
#1186=LINE('',#7436,#1641);
#1187=LINE('',#7443,#1642);
#1188=LINE('',#7445,#1643);
#1189=LINE('',#7446,#1644);
#1190=LINE('',#7451,#1645);
#1191=LINE('',#7455,#1646);
#1192=LINE('',#7457,#1647);
#1193=LINE('',#7458,#1648);
#1194=LINE('',#7463,#1649);
#1195=LINE('',#7468,#1650);
#1196=LINE('',#7487,#1651);
#1197=LINE('',#7492,#1652);
#1198=LINE('',#7494,#1653);
#1199=LINE('',#7497,#1654);
#1200=LINE('',#7500,#1655);
#1201=LINE('',#7514,#1656);
#1202=LINE('',#7526,#1657);
#1203=LINE('',#7529,#1658);
#1204=LINE('',#7535,#1659);
#1205=LINE('',#7537,#1660);
#1206=LINE('',#7539,#1661);
#1207=LINE('',#7540,#1662);
#1208=LINE('',#7544,#1663);
#1209=LINE('',#7546,#1664);
#1210=LINE('',#7548,#1665);
#1211=LINE('',#7549,#1666);
#1212=LINE('',#7551,#1667);
#1213=LINE('',#7552,#1668);
#1214=LINE('',#7555,#1669);
#1215=LINE('',#7557,#1670);
#1216=LINE('',#7559,#1671);
#1217=LINE('',#7561,#1672);
#1218=LINE('',#7563,#1673);
#1219=LINE('',#7565,#1674);
#1220=LINE('',#7566,#1675);
#1221=LINE('',#7569,#1676);
#1222=LINE('',#7571,#1677);
#1223=LINE('',#7573,#1678);
#1224=LINE('',#7575,#1679);
#1225=LINE('',#7577,#1680);
#1226=LINE('',#7579,#1681);
#1227=LINE('',#7580,#1682);
#1228=LINE('',#7583,#1683);
#1229=LINE('',#7585,#1684);
#1230=LINE('',#7586,#1685);
#1231=LINE('',#7590,#1686);
#1232=LINE('',#7592,#1687);
#1233=LINE('',#7594,#1688);
#1234=LINE('',#7595,#1689);
#1235=LINE('',#7598,#1690);
#1236=LINE('',#7600,#1691);
#1237=LINE('',#7601,#1692);
#1238=LINE('',#7605,#1693);
#1239=LINE('',#7606,#1694);
#1240=LINE('',#7607,#1695);
#1241=LINE('',#7610,#1696);
#1242=LINE('',#7611,#1697);
#1243=LINE('',#7614,#1698);
#1244=LINE('',#7616,#1699);
#1245=LINE('',#7618,#1700);
#1246=LINE('',#7619,#1701);
#1247=LINE('',#7622,#1702);
#1248=LINE('',#7624,#1703);
#1249=LINE('',#7626,#1704);
#1250=LINE('',#7627,#1705);
#1251=LINE('',#7630,#1706);
#1252=LINE('',#7632,#1707);
#1253=LINE('',#7634,#1708);
#1254=LINE('',#7635,#1709);
#1255=LINE('',#7638,#1710);
#1256=LINE('',#7640,#1711);
#1257=LINE('',#7642,#1712);
#1258=LINE('',#7643,#1713);
#1259=LINE('',#7646,#1714);
#1260=LINE('',#7648,#1715);
#1261=LINE('',#7650,#1716);
#1262=LINE('',#7651,#1717);
#1263=LINE('',#7654,#1718);
#1264=LINE('',#7656,#1719);
#1265=LINE('',#7658,#1720);
#1266=LINE('',#7659,#1721);
#1267=LINE('',#7662,#1722);
#1268=LINE('',#7664,#1723);
#1269=LINE('',#7666,#1724);
#1270=LINE('',#7667,#1725);
#1271=LINE('',#7670,#1726);
#1272=LINE('',#7672,#1727);
#1273=LINE('',#7674,#1728);
#1274=LINE('',#7675,#1729);
#1275=LINE('',#7681,#1730);
#1276=LINE('',#7682,#1731);
#1277=LINE('',#7686,#1732);
#1278=LINE('',#7689,#1733);
#1279=LINE('',#7695,#1734);
#1280=LINE('',#7696,#1735);
#1281=LINE('',#7700,#1736);
#1282=LINE('',#7703,#1737);
#1283=LINE('',#7709,#1738);
#1284=LINE('',#7710,#1739);
#1285=LINE('',#7716,#1740);
#1286=LINE('',#7717,#1741);
#1287=LINE('',#7720,#1742);
#1288=LINE('',#7722,#1743);
#1289=LINE('',#7723,#1744);
#1290=LINE('',#7727,#1745);
#1291=LINE('',#7730,#1746);
#1292=LINE('',#7736,#1747);
#1293=LINE('',#7737,#1748);
#1294=LINE('',#7741,#1749);
#1295=LINE('',#7744,#1750);
#1296=LINE('',#7748,#1751);
#1297=LINE('',#7749,#1752);
#1298=LINE('',#7750,#1753);
#1299=LINE('',#7751,#1754);
#1300=LINE('',#7752,#1755);
#1301=LINE('',#7753,#1756);
#1302=LINE('',#7755,#1757);
#1303=LINE('',#7756,#1758);
#1304=LINE('',#7757,#1759);
#1305=LINE('',#7759,#1760);
#1306=LINE('',#7761,#1761);
#1307=LINE('',#7762,#1762);
#1308=LINE('',#7764,#1763);
#1309=LINE('',#7765,#1764);
#1310=LINE('',#7768,#1765);
#1311=LINE('',#7769,#1766);
#1312=LINE('',#7772,#1767);
#1313=LINE('',#7774,#1768);
#1314=LINE('',#7776,#1769);
#1315=LINE('',#7777,#1770);
#1316=LINE('',#7780,#1771);
#1317=LINE('',#7782,#1772);
#1318=LINE('',#7784,#1773);
#1319=LINE('',#7785,#1774);
#1320=LINE('',#7788,#1775);
#1321=LINE('',#7790,#1776);
#1322=LINE('',#7792,#1777);
#1323=LINE('',#7793,#1778);
#1324=LINE('',#7796,#1779);
#1325=LINE('',#7798,#1780);
#1326=LINE('',#7800,#1781);
#1327=LINE('',#7801,#1782);
#1328=LINE('',#7804,#1783);
#1329=LINE('',#7806,#1784);
#1330=LINE('',#7808,#1785);
#1331=LINE('',#7809,#1786);
#1332=LINE('',#7812,#1787);
#1333=LINE('',#7814,#1788);
#1334=LINE('',#7816,#1789);
#1335=LINE('',#7817,#1790);
#1336=LINE('',#7820,#1791);
#1337=LINE('',#7822,#1792);
#1338=LINE('',#7824,#1793);
#1339=LINE('',#7825,#1794);
#1340=LINE('',#7828,#1795);
#1341=LINE('',#7830,#1796);
#1342=LINE('',#7832,#1797);
#1343=LINE('',#7833,#1798);
#1344=LINE('',#7839,#1799);
#1345=LINE('',#7840,#1800);
#1346=LINE('',#7844,#1801);
#1347=LINE('',#7847,#1802);
#1348=LINE('',#7851,#1803);
#1349=LINE('',#7854,#1804);
#1350=LINE('',#7858,#1805);
#1351=LINE('',#7860,#1806);
#1352=LINE('',#7862,#1807);
#1353=LINE('',#7863,#1808);
#1354=LINE('',#7867,#1809);
#1355=LINE('',#7869,#1810);
#1356=LINE('',#7871,#1811);
#1357=LINE('',#7872,#1812);
#1358=LINE('',#7876,#1813);
#1359=LINE('',#7878,#1814);
#1360=LINE('',#7880,#1815);
#1361=LINE('',#7881,#1816);
#1362=LINE('',#7887,#1817);
#1363=LINE('',#7888,#1818);
#1364=LINE('',#7892,#1819);
#1365=LINE('',#7895,#1820);
#1366=LINE('',#7899,#1821);
#1367=LINE('',#7901,#1822);
#1368=LINE('',#7903,#1823);
#1369=LINE('',#7904,#1824);
#1370=LINE('',#7906,#1825);
#1371=LINE('',#7907,#1826);
#1372=LINE('',#7910,#1827);
#1373=LINE('',#7912,#1828);
#1374=LINE('',#7913,#1829);
#1375=LINE('',#7915,#1830);
#1376=LINE('',#7916,#1831);
#1377=LINE('',#7920,#1832);
#1378=LINE('',#7922,#1833);
#1379=LINE('',#7923,#1834);
#1380=LINE('',#7925,#1835);
#1381=LINE('',#7927,#1836);
#1382=LINE('',#7928,#1837);
#1383=LINE('',#7930,#1838);
#1384=LINE('',#7932,#1839);
#1385=LINE('',#7933,#1840);
#1386=LINE('',#7935,#1841);
#1387=LINE('',#7937,#1842);
#1388=LINE('',#7938,#1843);
#1389=LINE('',#7940,#1844);
#1390=LINE('',#7942,#1845);
#1391=LINE('',#7944,#1846);
#1392=LINE('',#7945,#1847);
#1393=LINE('',#7948,#1848);
#1394=LINE('',#7950,#1849);
#1395=LINE('',#7951,#1850);
#1396=LINE('',#7955,#1851);
#1397=LINE('',#7956,#1852);
#1398=LINE('',#7957,#1853);
#1399=LINE('',#7958,#1854);
#1400=LINE('',#7962,#1855);
#1401=LINE('',#7964,#1856);
#1402=LINE('',#7966,#1857);
#1403=LINE('',#7967,#1858);
#1404=LINE('',#7971,#1859);
#1405=LINE('',#7973,#1860);
#1406=LINE('',#7975,#1861);
#1407=LINE('',#7977,#1862);
#1408=LINE('',#7990,#1863);
#1409=LINE('',#7995,#1864);
#1410=LINE('',#7997,#1865);
#1411=LINE('',#8011,#1866);
#1412=LINE('',#8013,#1867);
#1413=LINE('',#8016,#1868);
#1414=LINE('',#8018,#1869);
#1415=LINE('',#8020,#1870);
#1416=LINE('',#8022,#1871);
#1417=LINE('',#8024,#1872);
#1418=LINE('',#8026,#1873);
#1419=LINE('',#8027,#1874);
#1420=LINE('',#8031,#1875);
#1421=LINE('',#8045,#1876);
#1422=LINE('',#8046,#1877);
#1423=LINE('',#8049,#1878);
#1424=LINE('',#8051,#1879);
#1425=LINE('',#8052,#1880);
#1426=LINE('',#8056,#1881);
#1427=LINE('',#8066,#1882);
#1428=LINE('',#8067,#1883);
#1429=LINE('',#8068,#1884);
#1430=LINE('',#8069,#1885);
#1431=LINE('',#8070,#1886);
#1432=LINE('',#8076,#1887);
#1433=LINE('',#8079,#1888);
#1434=LINE('',#8084,#1889);
#1435=LINE('',#8087,#1890);
#1436=LINE('',#8090,#1891);
#1437=LINE('',#8094,#1892);
#1438=LINE('',#8098,#1893);
#1439=LINE('',#8102,#1894);
#1440=LINE('',#8106,#1895);
#1441=LINE('',#8110,#1896);
#1442=LINE('',#8114,#1897);
#1443=LINE('',#8118,#1898);
#1444=LINE('',#8124,#1899);
#1445=LINE('',#8127,#1900);
#1446=LINE('',#8130,#1901);
#1447=LINE('',#8134,#1902);
#1448=LINE('',#8140,#1903);
#1449=LINE('',#8142,#1904);
#1450=LINE('',#8148,#1905);
#1451=LINE('',#8149,#1906);
#1452=LINE('',#8162,#1907);
#1453=LINE('',#8164,#1908);
#1454=LINE('',#8173,#1909);
#1455=LINE('',#8175,#1910);
#1456=LINE('',#8184,#1911);
#1457=LINE('',#8186,#1912);
#1458=LINE('',#8195,#1913);
#1459=LINE('',#8197,#1914);
#1460=LINE('',#8203,#1915);
#1461=LINE('',#8204,#1916);
#1462=LINE('',#8214,#1917);
#1463=LINE('',#8215,#1918);
#1464=LINE('',#8225,#1919);
#1465=LINE('',#8228,#1920);
#1466=LINE('',#8231,#1921);
#1467=LINE('',#8234,#1922);
#1468=LINE('',#8237,#1923);
#1469=LINE('',#8240,#1924);
#1470=LINE('',#8243,#1925);
#1471=LINE('',#8246,#1926);
#1472=LINE('',#8253,#1927);
#1473=LINE('',#8254,#1928);
#1474=LINE('',#8257,#1929);
#1475=LINE('',#8259,#1930);
#1476=LINE('',#8260,#1931);
#1477=LINE('',#8264,#1932);
#1478=LINE('',#8267,#1933);
#1479=LINE('',#8269,#1934);
#1480=LINE('',#8270,#1935);
#1481=LINE('',#8274,#1936);
#1482=LINE('',#8282,#1937);
#1483=LINE('',#8283,#1938);
#1484=LINE('',#8285,#1939);
#1485=LINE('',#8286,#1940);
#1486=LINE('',#8292,#1941);
#1487=LINE('',#8293,#1942);
#1488=LINE('',#8296,#1943);
#1489=LINE('',#8298,#1944);
#1490=LINE('',#8299,#1945);
#1491=LINE('',#8303,#1946);
#1492=LINE('',#8305,#1947);
#1493=LINE('',#8307,#1948);
#1494=LINE('',#8309,#1949);
#1495=LINE('',#8311,#1950);
#1496=LINE('',#8312,#1951);
#1497=LINE('',#8313,#1952);
#1498=LINE('',#8314,#1953);
#1499=LINE('',#8315,#1954);
#1500=LINE('',#8321,#1955);
#1501=LINE('',#8324,#1956);
#1502=LINE('',#8327,#1957);
#1503=LINE('',#8331,#1958);
#1504=LINE('',#8335,#1959);
#1505=LINE('',#8339,#1960);
#1506=LINE('',#8343,#1961);
#1507=LINE('',#8347,#1962);
#1508=LINE('',#8351,#1963);
#1509=LINE('',#8355,#1964);
#1510=LINE('',#8361,#1965);
#1511=LINE('',#8364,#1966);
#1512=LINE('',#8367,#1967);
#1513=LINE('',#8371,#1968);
#1514=LINE('',#8377,#1969);
#1515=LINE('',#8380,#1970);
#1516=LINE('',#8382,#1971);
#1517=LINE('',#8383,#1972);
#1518=LINE('',#8388,#1973);
#1519=LINE('',#8393,#1974);
#1520=LINE('',#8394,#1975);
#1521=LINE('',#8395,#1976);
#1522=LINE('',#8402,#1977);
#1523=LINE('',#8404,#1978);
#1524=LINE('',#8406,#1979);
#1525=LINE('',#8407,#1980);
#1526=LINE('',#8410,#1981);
#1527=LINE('',#8413,#1982);
#1528=LINE('',#8418,#1983);
#1529=LINE('',#8419,#1984);
#1530=LINE('',#8424,#1985);
#1531=LINE('',#8429,#1986);
#1532=LINE('',#8430,#1987);
#1533=LINE('',#8431,#1988);
#1534=LINE('',#8438,#1989);
#1535=LINE('',#8440,#1990);
#1536=LINE('',#8442,#1991);
#1537=LINE('',#8443,#1992);
#1538=LINE('',#8446,#1993);
#1539=LINE('',#8449,#1994);
#1540=LINE('',#8456,#1995);
#1541=LINE('',#8458,#1996);
#1542=LINE('',#8460,#1997);
#1543=LINE('',#8461,#1998);
#1544=LINE('',#8464,#1999);
#1545=LINE('',#8467,#2000);
#1546=LINE('',#8474,#2001);
#1547=LINE('',#8476,#2002);
#1548=LINE('',#8478,#2003);
#1549=LINE('',#8479,#2004);
#1550=LINE('',#8482,#2005);
#1551=LINE('',#8485,#2006);
#1552=LINE('',#8492,#2007);
#1553=LINE('',#8494,#2008);
#1554=LINE('',#8496,#2009);
#1555=LINE('',#8497,#2010);
#1556=LINE('',#8500,#2011);
#1557=LINE('',#8503,#2012);
#1558=LINE('',#8508,#2013);
#1559=LINE('',#8509,#2014);
#1560=LINE('',#8514,#2015);
#1561=LINE('',#8519,#2016);
#1562=LINE('',#8520,#2017);
#1563=LINE('',#8521,#2018);
#1564=LINE('',#8548,#2019);
#1565=LINE('',#8552,#2020);
#1566=LINE('',#8556,#2021);
#1567=LINE('',#8560,#2022);
#1568=LINE('',#8566,#2023);
#1569=LINE('',#8571,#2024);
#1570=LINE('',#8575,#2025);
#1571=LINE('',#8576,#2026);
#1572=LINE('',#8577,#2027);
#1573=LINE('',#8580,#2028);
#1574=LINE('',#8582,#2029);
#1575=LINE('',#8583,#2030);
#1576=LINE('',#8586,#2031);
#1577=LINE('',#8588,#2032);
#1578=LINE('',#8589,#2033);
#1579=LINE('',#8596,#2034);
#1580=LINE('',#8598,#2035);
#1581=LINE('',#8599,#2036);
#1582=LINE('',#8604,#2037);
#1583=LINE('',#8608,#2038);
#1584=LINE('',#8610,#2039);
#1585=LINE('',#8611,#2040);
#1586=LINE('',#8616,#2041);
#1587=LINE('',#8621,#2042);
#1588=LINE('',#8640,#2043);
#1589=LINE('',#8643,#2044);
#1590=LINE('',#8645,#2045);
#1591=LINE('',#8650,#2046);
#1592=LINE('',#8653,#2047);
#1593=LINE('',#8667,#2048);
#1594=LINE('',#8679,#2049);
#1595=LINE('',#8682,#2050);
#1596=LINE('',#8690,#2051);
#1597=LINE('',#8715,#2052);
#1598=LINE('',#8720,#2053);
#1599=LINE('',#8727,#2054);
#1600=LINE('',#8735,#2055);
#1601=LINE('',#8741,#2056);
#1602=LINE('',#8746,#2057);
#1603=LINE('',#8752,#2058);
#1604=LINE('',#8761,#2059);
#1605=LINE('',#8766,#2060);
#1606=LINE('',#8770,#2061);
#1607=LINE('',#8778,#2062);
#1608=LINE('',#8785,#2063);
#1609=LINE('',#8789,#2064);
#1610=LINE('',#8793,#2065);
#1611=LINE('',#8796,#2066);
#1612=LINE('',#8801,#2067);
#1613=LINE('',#8808,#2068);
#1614=LINE('',#8816,#2069);
#1615=LINE('',#8823,#2070);
#1616=LINE('',#8830,#2071);
#1617=LINE('',#8841,#2072);
#1618=LINE('',#8848,#2073);
#1619=LINE('',#8852,#2074);
#1620=LINE('',#8857,#2075);
#1621=LINE('',#8866,#2076);
#1622=LINE('',#8872,#2077);
#1623=LINE('',#8881,#2078);
#1624=LINE('',#8889,#2079);
#1625=LINE('',#8892,#2080);
#1626=LINE('',#8898,#2081);
#1627=VECTOR('',#5823,0.01);
#1628=VECTOR('',#5826,0.01);
#1629=VECTOR('',#5829,0.01);
#1630=VECTOR('',#5832,0.01);
#1631=VECTOR('',#5835,0.01);
#1632=VECTOR('',#5840,0.01);
#1633=VECTOR('',#5847,1.);
#1634=VECTOR('',#5848,1.);
#1635=VECTOR('',#5849,1.);
#1636=VECTOR('',#5852,1.);
#1637=VECTOR('',#5853,1.);
#1638=VECTOR('',#5854,0.01);
#1639=VECTOR('',#5857,1.);
#1640=VECTOR('',#5858,1.);
#1641=VECTOR('',#5859,0.01);
#1642=VECTOR('',#5866,1.);
#1643=VECTOR('',#5867,1.);
#1644=VECTOR('',#5868,0.01);
#1645=VECTOR('',#5873,0.004225);
#1646=VECTOR('',#5878,1.);
#1647=VECTOR('',#5879,1.);
#1648=VECTOR('',#5880,0.01);
#1649=VECTOR('',#5885,0.004225);
#1650=VECTOR('',#5890,1.);
#1651=VECTOR('',#5921,0.01);
#1652=VECTOR('',#5926,1.);
#1653=VECTOR('',#5927,1.);
#1654=VECTOR('',#5930,0.01);
#1655=VECTOR('',#5933,0.007625);
#1656=VECTOR('',#5936,0.007625);
#1657=VECTOR('',#5939,0.01);
#1658=VECTOR('',#5944,0.01);
#1659=VECTOR('',#5951,0.01);
#1660=VECTOR('',#5952,0.01);
#1661=VECTOR('',#5953,0.01);
#1662=VECTOR('',#5954,0.01);
#1663=VECTOR('',#5957,0.01);
#1664=VECTOR('',#5958,0.01);
#1665=VECTOR('',#5959,0.01);
#1666=VECTOR('',#5960,0.01);
#1667=VECTOR('',#5963,0.01);
#1668=VECTOR('',#5964,0.01);
#1669=VECTOR('',#5967,1.);
#1670=VECTOR('',#5968,1.);
#1671=VECTOR('',#5969,1.);
#1672=VECTOR('',#5970,1.);
#1673=VECTOR('',#5971,1.);
#1674=VECTOR('',#5972,1.);
#1675=VECTOR('',#5973,1.);
#1676=VECTOR('',#5976,1.);
#1677=VECTOR('',#5977,1.);
#1678=VECTOR('',#5978,1.);
#1679=VECTOR('',#5979,1.);
#1680=VECTOR('',#5980,1.);
#1681=VECTOR('',#5981,1.);
#1682=VECTOR('',#5982,1.);
#1683=VECTOR('',#5985,1.);
#1684=VECTOR('',#5986,1.);
#1685=VECTOR('',#5987,1.);
#1686=VECTOR('',#5990,0.01);
#1687=VECTOR('',#5991,0.01);
#1688=VECTOR('',#5992,0.01);
#1689=VECTOR('',#5993,1.);
#1690=VECTOR('',#5996,0.01);
#1691=VECTOR('',#5997,0.01);
#1692=VECTOR('',#5998,0.01);
#1693=VECTOR('',#6001,0.01);
#1694=VECTOR('',#6002,0.01);
#1695=VECTOR('',#6003,0.01);
#1696=VECTOR('',#6006,1.);
#1697=VECTOR('',#6007,1.);
#1698=VECTOR('',#6008,1.);
#1699=VECTOR('',#6009,1.);
#1700=VECTOR('',#6010,1.);
#1701=VECTOR('',#6011,1.);
#1702=VECTOR('',#6012,1.);
#1703=VECTOR('',#6013,1.);
#1704=VECTOR('',#6014,1.);
#1705=VECTOR('',#6015,1.);
#1706=VECTOR('',#6016,1.);
#1707=VECTOR('',#6017,1.);
#1708=VECTOR('',#6018,1.);
#1709=VECTOR('',#6019,1.);
#1710=VECTOR('',#6020,1.);
#1711=VECTOR('',#6021,1.);
#1712=VECTOR('',#6022,1.);
#1713=VECTOR('',#6023,1.);
#1714=VECTOR('',#6024,1.);
#1715=VECTOR('',#6025,1.);
#1716=VECTOR('',#6026,1.);
#1717=VECTOR('',#6027,1.);
#1718=VECTOR('',#6028,1.);
#1719=VECTOR('',#6029,1.);
#1720=VECTOR('',#6030,1.);
#1721=VECTOR('',#6031,1.);
#1722=VECTOR('',#6032,1.);
#1723=VECTOR('',#6033,1.);
#1724=VECTOR('',#6034,1.);
#1725=VECTOR('',#6035,1.);
#1726=VECTOR('',#6036,1.);
#1727=VECTOR('',#6037,1.);
#1728=VECTOR('',#6038,1.);
#1729=VECTOR('',#6039,1.);
#1730=VECTOR('',#6044,1.);
#1731=VECTOR('',#6045,1.);
#1732=VECTOR('',#6048,1.);
#1733=VECTOR('',#6051,1.);
#1734=VECTOR('',#6056,1.);
#1735=VECTOR('',#6057,1.);
#1736=VECTOR('',#6060,1.);
#1737=VECTOR('',#6063,1.);
#1738=VECTOR('',#6068,1.);
#1739=VECTOR('',#6069,1.);
#1740=VECTOR('',#6074,1.);
#1741=VECTOR('',#6075,1.);
#1742=VECTOR('',#6078,1.);
#1743=VECTOR('',#6079,1.);
#1744=VECTOR('',#6080,1.);
#1745=VECTOR('',#6083,1.);
#1746=VECTOR('',#6086,1.);
#1747=VECTOR('',#6091,1.);
#1748=VECTOR('',#6092,1.);
#1749=VECTOR('',#6095,1.);
#1750=VECTOR('',#6098,1.);
#1751=VECTOR('',#6101,1.);
#1752=VECTOR('',#6102,1.);
#1753=VECTOR('',#6103,1.);
#1754=VECTOR('',#6104,1.);
#1755=VECTOR('',#6105,1.);
#1756=VECTOR('',#6106,1.);
#1757=VECTOR('',#6107,1.);
#1758=VECTOR('',#6108,1.);
#1759=VECTOR('',#6109,1.);
#1760=VECTOR('',#6110,1.);
#1761=VECTOR('',#6111,1.);
#1762=VECTOR('',#6112,1.);
#1763=VECTOR('',#6115,1.);
#1764=VECTOR('',#6116,1.);
#1765=VECTOR('',#6119,1.);
#1766=VECTOR('',#6120,1.);
#1767=VECTOR('',#6121,1.);
#1768=VECTOR('',#6122,1.);
#1769=VECTOR('',#6123,1.);
#1770=VECTOR('',#6124,1.);
#1771=VECTOR('',#6125,1.);
#1772=VECTOR('',#6126,1.);
#1773=VECTOR('',#6127,1.);
#1774=VECTOR('',#6128,1.);
#1775=VECTOR('',#6129,1.);
#1776=VECTOR('',#6130,1.);
#1777=VECTOR('',#6131,1.);
#1778=VECTOR('',#6132,1.);
#1779=VECTOR('',#6133,1.);
#1780=VECTOR('',#6134,1.);
#1781=VECTOR('',#6135,1.);
#1782=VECTOR('',#6136,1.);
#1783=VECTOR('',#6137,1.);
#1784=VECTOR('',#6138,1.);
#1785=VECTOR('',#6139,1.);
#1786=VECTOR('',#6140,1.);
#1787=VECTOR('',#6141,1.);
#1788=VECTOR('',#6142,1.);
#1789=VECTOR('',#6143,1.);
#1790=VECTOR('',#6144,1.);
#1791=VECTOR('',#6145,1.);
#1792=VECTOR('',#6146,1.);
#1793=VECTOR('',#6147,1.);
#1794=VECTOR('',#6148,1.);
#1795=VECTOR('',#6149,1.);
#1796=VECTOR('',#6150,1.);
#1797=VECTOR('',#6151,1.);
#1798=VECTOR('',#6152,1.);
#1799=VECTOR('',#6157,1.);
#1800=VECTOR('',#6158,1.);
#1801=VECTOR('',#6161,1.);
#1802=VECTOR('',#6164,1.);
#1803=VECTOR('',#6167,1.);
#1804=VECTOR('',#6170,1.);
#1805=VECTOR('',#6173,1.);
#1806=VECTOR('',#6174,1.);
#1807=VECTOR('',#6175,1.);
#1808=VECTOR('',#6176,1.);
#1809=VECTOR('',#6179,1.);
#1810=VECTOR('',#6180,1.);
#1811=VECTOR('',#6181,1.);
#1812=VECTOR('',#6182,1.);
#1813=VECTOR('',#6185,1.);
#1814=VECTOR('',#6186,1.);
#1815=VECTOR('',#6187,1.);
#1816=VECTOR('',#6188,1.);
#1817=VECTOR('',#6193,1.);
#1818=VECTOR('',#6194,1.);
#1819=VECTOR('',#6197,1.);
#1820=VECTOR('',#6200,1.);
#1821=VECTOR('',#6203,1.);
#1822=VECTOR('',#6204,1.);
#1823=VECTOR('',#6205,1.);
#1824=VECTOR('',#6206,1.);
#1825=VECTOR('',#6209,1.);
#1826=VECTOR('',#6210,1.);
#1827=VECTOR('',#6213,1.);
#1828=VECTOR('',#6214,1.);
#1829=VECTOR('',#6215,1.);
#1830=VECTOR('',#6218,1.);
#1831=VECTOR('',#6219,1.);
#1832=VECTOR('',#6222,1.);
#1833=VECTOR('',#6223,1.);
#1834=VECTOR('',#6224,1.);
#1835=VECTOR('',#6225,1.);
#1836=VECTOR('',#6226,1.);
#1837=VECTOR('',#6227,1.);
#1838=VECTOR('',#6228,1.);
#1839=VECTOR('',#6229,1.);
#1840=VECTOR('',#6230,1.);
#1841=VECTOR('',#6231,1.);
#1842=VECTOR('',#6232,1.);
#1843=VECTOR('',#6233,1.);
#1844=VECTOR('',#6234,1.);
#1845=VECTOR('',#6235,1.);
#1846=VECTOR('',#6236,1.);
#1847=VECTOR('',#6237,1.);
#1848=VECTOR('',#6240,1.);
#1849=VECTOR('',#6241,1.);
#1850=VECTOR('',#6242,1.);
#1851=VECTOR('',#6245,1.);
#1852=VECTOR('',#6246,1.);
#1853=VECTOR('',#6247,1.);
#1854=VECTOR('',#6248,1.);
#1855=VECTOR('',#6253,1.);
#1856=VECTOR('',#6254,1.);
#1857=VECTOR('',#6255,1.);
#1858=VECTOR('',#6256,1.);
#1859=VECTOR('',#6259,1.);
#1860=VECTOR('',#6260,1.);
#1861=VECTOR('',#6263,1.);
#1862=VECTOR('',#6266,1.);
#1863=VECTOR('',#6279,1.);
#1864=VECTOR('',#6284,1.);
#1865=VECTOR('',#6285,1.);
#1866=VECTOR('',#6302,1.);
#1867=VECTOR('',#6305,1.);
#1868=VECTOR('',#6310,0.0125);
#1869=VECTOR('',#6313,0.00123);
#1870=VECTOR('',#6316,0.00123);
#1871=VECTOR('',#6319,0.00123);
#1872=VECTOR('',#6322,0.00123);
#1873=VECTOR('',#6325,1.);
#1874=VECTOR('',#6326,1.);
#1875=VECTOR('',#6331,1.);
#1876=VECTOR('',#6352,1.);
#1877=VECTOR('',#6353,1.);
#1878=VECTOR('',#6356,1.);
#1879=VECTOR('',#6357,1.);
#1880=VECTOR('',#6358,1.);
#1881=VECTOR('',#6363,1.);
#1882=VECTOR('',#6382,1.);
#1883=VECTOR('',#6383,1.);
#1884=VECTOR('',#6384,1.);
#1885=VECTOR('',#6385,1.);
#1886=VECTOR('',#6386,1.);
#1887=VECTOR('',#6391,1.);
#1888=VECTOR('',#6394,1.);
#1889=VECTOR('',#6397,1.);
#1890=VECTOR('',#6400,1.);
#1891=VECTOR('',#6401,1.);
#1892=VECTOR('',#6404,1.);
#1893=VECTOR('',#6407,1.);
#1894=VECTOR('',#6410,1.);
#1895=VECTOR('',#6413,1.);
#1896=VECTOR('',#6416,1.);
#1897=VECTOR('',#6419,1.);
#1898=VECTOR('',#6422,1.);
#1899=VECTOR('',#6427,1.);
#1900=VECTOR('',#6430,1.);
#1901=VECTOR('',#6431,1.);
#1902=VECTOR('',#6434,1.);
#1903=VECTOR('',#6443,1.);
#1904=VECTOR('',#6446,1.);
#1905=VECTOR('',#6455,1.);
#1906=VECTOR('',#6456,1.);
#1907=VECTOR('',#6475,1.);
#1908=VECTOR('',#6478,1.);
#1909=VECTOR('',#6491,1.);
#1910=VECTOR('',#6494,1.);
#1911=VECTOR('',#6507,1.);
#1912=VECTOR('',#6510,1.);
#1913=VECTOR('',#6523,1.);
#1914=VECTOR('',#6526,1.);
#1915=VECTOR('',#6535,1.);
#1916=VECTOR('',#6536,1.);
#1917=VECTOR('',#6551,1.);
#1918=VECTOR('',#6552,1.);
#1919=VECTOR('',#6567,1.);
#1920=VECTOR('',#6572,1.);
#1921=VECTOR('',#6577,1.);
#1922=VECTOR('',#6582,1.);
#1923=VECTOR('',#6587,1.);
#1924=VECTOR('',#6592,1.);
#1925=VECTOR('',#6597,1.);
#1926=VECTOR('',#6602,1.);
#1927=VECTOR('',#6609,1.);
#1928=VECTOR('',#6610,1.);
#1929=VECTOR('',#6613,1.);
#1930=VECTOR('',#6614,1.);
#1931=VECTOR('',#6615,1.);
#1932=VECTOR('',#6620,1.);
#1933=VECTOR('',#6623,1.);
#1934=VECTOR('',#6624,1.);
#1935=VECTOR('',#6625,1.);
#1936=VECTOR('',#6630,1.);
#1937=VECTOR('',#6639,1.);
#1938=VECTOR('',#6640,1.);
#1939=VECTOR('',#6643,1.);
#1940=VECTOR('',#6644,1.);
#1941=VECTOR('',#6649,1.);
#1942=VECTOR('',#6650,1.);
#1943=VECTOR('',#6653,1.);
#1944=VECTOR('',#6654,1.);
#1945=VECTOR('',#6655,1.);
#1946=VECTOR('',#6660,1.);
#1947=VECTOR('',#6663,1.);
#1948=VECTOR('',#6666,1.);
#1949=VECTOR('',#6669,1.);
#1950=VECTOR('',#6672,1.);
#1951=VECTOR('',#6673,1.);
#1952=VECTOR('',#6674,1.);
#1953=VECTOR('',#6675,1.);
#1954=VECTOR('',#6676,1.);
#1955=VECTOR('',#6681,1.);
#1956=VECTOR('',#6684,1.);
#1957=VECTOR('',#6685,1.);
#1958=VECTOR('',#6688,1.);
#1959=VECTOR('',#6691,1.);
#1960=VECTOR('',#6694,1.);
#1961=VECTOR('',#6697,1.);
#1962=VECTOR('',#6700,1.);
#1963=VECTOR('',#6703,1.);
#1964=VECTOR('',#6706,1.);
#1965=VECTOR('',#6711,1.);
#1966=VECTOR('',#6714,1.);
#1967=VECTOR('',#6715,1.);
#1968=VECTOR('',#6718,1.);
#1969=VECTOR('',#6723,1.);
#1970=VECTOR('',#6726,1.);
#1971=VECTOR('',#6729,1.);
#1972=VECTOR('',#6730,1.);
#1973=VECTOR('',#6735,1.);
#1974=VECTOR('',#6740,1.);
#1975=VECTOR('',#6741,1.);
#1976=VECTOR('',#6742,1.);
#1977=VECTOR('',#6751,1.);
#1978=VECTOR('',#6752,1.);
#1979=VECTOR('',#6753,1.);
#1980=VECTOR('',#6754,1.);
#1981=VECTOR('',#6759,1.);
#1982=VECTOR('',#6764,1.);
#1983=VECTOR('',#6773,1.);
#1984=VECTOR('',#6774,1.);
#1985=VECTOR('',#6779,1.);
#1986=VECTOR('',#6784,1.);
#1987=VECTOR('',#6785,1.);
#1988=VECTOR('',#6786,1.);
#1989=VECTOR('',#6795,1.);
#1990=VECTOR('',#6796,1.);
#1991=VECTOR('',#6797,1.);
#1992=VECTOR('',#6798,1.);
#1993=VECTOR('',#6803,1.);
#1994=VECTOR('',#6808,1.);
#1995=VECTOR('',#6817,1.);
#1996=VECTOR('',#6818,1.);
#1997=VECTOR('',#6819,1.);
#1998=VECTOR('',#6820,1.);
#1999=VECTOR('',#6825,1.);
#2000=VECTOR('',#6830,1.);
#2001=VECTOR('',#6839,1.);
#2002=VECTOR('',#6840,1.);
#2003=VECTOR('',#6841,1.);
#2004=VECTOR('',#6842,1.);
#2005=VECTOR('',#6847,1.);
#2006=VECTOR('',#6852,1.);
#2007=VECTOR('',#6861,1.);
#2008=VECTOR('',#6862,1.);
#2009=VECTOR('',#6863,1.);
#2010=VECTOR('',#6864,1.);
#2011=VECTOR('',#6869,1.);
#2012=VECTOR('',#6874,1.);
#2013=VECTOR('',#6883,1.);
#2014=VECTOR('',#6884,1.);
#2015=VECTOR('',#6889,1.);
#2016=VECTOR('',#6894,1.);
#2017=VECTOR('',#6895,1.);
#2018=VECTOR('',#6896,1.);
#2019=VECTOR('',#6943,0.01);
#2020=VECTOR('',#6946,0.01);
#2021=VECTOR('',#6949,0.01);
#2022=VECTOR('',#6952,0.01);
#2023=VECTOR('',#6957,0.01);
#2024=VECTOR('',#6962,0.01);
#2025=VECTOR('',#6965,1.);
#2026=VECTOR('',#6966,1.);
#2027=VECTOR('',#6967,1.);
#2028=VECTOR('',#6970,1.);
#2029=VECTOR('',#6971,1.);
#2030=VECTOR('',#6972,0.01);
#2031=VECTOR('',#6975,1.);
#2032=VECTOR('',#6976,1.);
#2033=VECTOR('',#6977,0.01);
#2034=VECTOR('',#6984,1.);
#2035=VECTOR('',#6985,1.);
#2036=VECTOR('',#6986,0.01);
#2037=VECTOR('',#6991,0.004225);
#2038=VECTOR('',#6996,1.);
#2039=VECTOR('',#6997,1.);
#2040=VECTOR('',#6998,0.01);
#2041=VECTOR('',#7003,0.004225);
#2042=VECTOR('',#7008,1.);
#2043=VECTOR('',#7039,0.01);
#2044=VECTOR('',#7042,1.);
#2045=VECTOR('',#7043,1.);
#2046=VECTOR('',#7048,0.01);
#2047=VECTOR('',#7051,0.007625);
#2048=VECTOR('',#7054,0.007625);
#2049=VECTOR('',#7057,0.01);
#2050=VECTOR('',#7062,0.01);
#2051=VECTOR('',#7071,0.004);
#2052=VECTOR('',#7108,0.007);
#2053=VECTOR('',#7115,0.0043);
#2054=VECTOR('',#7122,0.0066);
#2055=VECTOR('',#7133,0.0065);
#2056=VECTOR('',#7140,0.0074);
#2057=VECTOR('',#7147,0.0075);
#2058=VECTOR('',#7152,0.0066);
#2059=VECTOR('',#7165,0.0065);
#2060=VECTOR('',#7170,0.0074);
#2061=VECTOR('',#7175,0.0075);
#2062=VECTOR('',#7186,0.00700000010430813);
#2063=VECTOR('',#7195,0.0063);
#2064=VECTOR('',#7200,0.0061);
#2065=VECTOR('',#7205,0.0059);
#2066=VECTOR('',#7208,0.0061);
#2067=VECTOR('',#7215,0.0063);
#2068=VECTOR('',#7224,0.00700000010430813);
#2069=VECTOR('',#7235,0.00715);
#2070=VECTOR('',#7244,0.0075);
#2071=VECTOR('',#7253,0.00715);
#2072=VECTOR('',#7268,0.0065);
#2073=VECTOR('',#7277,0.0043);
#2074=VECTOR('',#7282,0.00405);
#2075=VECTOR('',#7289,0.0046499998960644);
#2076=VECTOR('',#7300,0.007);
#2077=VECTOR('',#7309,0.0043);
#2078=VECTOR('',#7320,0.0065);
#2079=VECTOR('',#7331,0.0043);
#2080=VECTOR('',#7334,0.00405);
#2081=VECTOR('',#7343,0.0046499998960644);
#2082=VERTEX_POINT('',#7391);
#2083=VERTEX_POINT('',#7392);
#2084=VERTEX_POINT('',#7394);
#2085=VERTEX_POINT('',#7396);
#2086=VERTEX_POINT('',#7398);
#2087=VERTEX_POINT('',#7400);
#2088=VERTEX_POINT('',#7402);
#2089=VERTEX_POINT('',#7404);
#2090=VERTEX_POINT('',#7406);
#2091=VERTEX_POINT('',#7408);
#2092=VERTEX_POINT('',#7410);
#2093=VERTEX_POINT('',#7412);
#2094=VERTEX_POINT('',#7414);
#2095=VERTEX_POINT('',#7416);
#2096=VERTEX_POINT('',#7420);
#2097=VERTEX_POINT('',#7421);
#2098=VERTEX_POINT('',#7426);
#2099=VERTEX_POINT('',#7428);
#2100=VERTEX_POINT('',#7432);
#2101=VERTEX_POINT('',#7434);
#2102=VERTEX_POINT('',#7437);
#2103=VERTEX_POINT('',#7439);
#2104=VERTEX_POINT('',#7442);
#2105=VERTEX_POINT('',#7444);
#2106=VERTEX_POINT('',#7448);
#2107=VERTEX_POINT('',#7450);
#2108=VERTEX_POINT('',#7454);
#2109=VERTEX_POINT('',#7456);
#2110=VERTEX_POINT('',#7460);
#2111=VERTEX_POINT('',#7462);
#2112=VERTEX_POINT('',#7466);
#2113=VERTEX_POINT('',#7467);
#2114=VERTEX_POINT('',#7469);
#2115=VERTEX_POINT('',#7476);
#2116=VERTEX_POINT('',#7486);
#2117=VERTEX_POINT('',#7488);
#2118=VERTEX_POINT('',#7490);
#2119=VERTEX_POINT('',#7493);
#2120=VERTEX_POINT('',#7495);
#2121=VERTEX_POINT('',#7499);
#2122=VERTEX_POINT('',#7533);
#2123=VERTEX_POINT('',#7534);
#2124=VERTEX_POINT('',#7536);
#2125=VERTEX_POINT('',#7538);
#2126=VERTEX_POINT('',#7542);
#2127=VERTEX_POINT('',#7543);
#2128=VERTEX_POINT('',#7545);
#2129=VERTEX_POINT('',#7547);
#2130=VERTEX_POINT('',#7554);
#2131=VERTEX_POINT('',#7556);
#2132=VERTEX_POINT('',#7558);
#2133=VERTEX_POINT('',#7560);
#2134=VERTEX_POINT('',#7562);
#2135=VERTEX_POINT('',#7564);
#2136=VERTEX_POINT('',#7568);
#2137=VERTEX_POINT('',#7570);
#2138=VERTEX_POINT('',#7572);
#2139=VERTEX_POINT('',#7574);
#2140=VERTEX_POINT('',#7576);
#2141=VERTEX_POINT('',#7578);
#2142=VERTEX_POINT('',#7582);
#2143=VERTEX_POINT('',#7584);
#2144=VERTEX_POINT('',#7588);
#2145=VERTEX_POINT('',#7589);
#2146=VERTEX_POINT('',#7591);
#2147=VERTEX_POINT('',#7593);
#2148=VERTEX_POINT('',#7597);
#2149=VERTEX_POINT('',#7599);
#2150=VERTEX_POINT('',#7603);
#2151=VERTEX_POINT('',#7604);
#2152=VERTEX_POINT('',#7609);
#2153=VERTEX_POINT('',#7612);
#2154=VERTEX_POINT('',#7613);
#2155=VERTEX_POINT('',#7615);
#2156=VERTEX_POINT('',#7617);
#2157=VERTEX_POINT('',#7620);
#2158=VERTEX_POINT('',#7621);
#2159=VERTEX_POINT('',#7623);
#2160=VERTEX_POINT('',#7625);
#2161=VERTEX_POINT('',#7628);
#2162=VERTEX_POINT('',#7629);
#2163=VERTEX_POINT('',#7631);
#2164=VERTEX_POINT('',#7633);
#2165=VERTEX_POINT('',#7636);
#2166=VERTEX_POINT('',#7637);
#2167=VERTEX_POINT('',#7639);
#2168=VERTEX_POINT('',#7641);
#2169=VERTEX_POINT('',#7644);
#2170=VERTEX_POINT('',#7645);
#2171=VERTEX_POINT('',#7647);
#2172=VERTEX_POINT('',#7649);
#2173=VERTEX_POINT('',#7652);
#2174=VERTEX_POINT('',#7653);
#2175=VERTEX_POINT('',#7655);
#2176=VERTEX_POINT('',#7657);
#2177=VERTEX_POINT('',#7660);
#2178=VERTEX_POINT('',#7661);
#2179=VERTEX_POINT('',#7663);
#2180=VERTEX_POINT('',#7665);
#2181=VERTEX_POINT('',#7668);
#2182=VERTEX_POINT('',#7669);
#2183=VERTEX_POINT('',#7671);
#2184=VERTEX_POINT('',#7673);
#2185=VERTEX_POINT('',#7677);
#2186=VERTEX_POINT('',#7678);
#2187=VERTEX_POINT('',#7680);
#2188=VERTEX_POINT('',#7684);
#2189=VERTEX_POINT('',#7685);
#2190=VERTEX_POINT('',#7687);
#2191=VERTEX_POINT('',#7691);
#2192=VERTEX_POINT('',#7692);
#2193=VERTEX_POINT('',#7694);
#2194=VERTEX_POINT('',#7698);
#2195=VERTEX_POINT('',#7699);
#2196=VERTEX_POINT('',#7701);
#2197=VERTEX_POINT('',#7705);
#2198=VERTEX_POINT('',#7706);
#2199=VERTEX_POINT('',#7708);
#2200=VERTEX_POINT('',#7712);
#2201=VERTEX_POINT('',#7713);
#2202=VERTEX_POINT('',#7715);
#2203=VERTEX_POINT('',#7719);
#2204=VERTEX_POINT('',#7721);
#2205=VERTEX_POINT('',#7725);
#2206=VERTEX_POINT('',#7726);
#2207=VERTEX_POINT('',#7728);
#2208=VERTEX_POINT('',#7732);
#2209=VERTEX_POINT('',#7733);
#2210=VERTEX_POINT('',#7735);
#2211=VERTEX_POINT('',#7739);
#2212=VERTEX_POINT('',#7740);
#2213=VERTEX_POINT('',#7742);
#2214=VERTEX_POINT('',#7746);
#2215=VERTEX_POINT('',#7747);
#2216=VERTEX_POINT('',#7754);
#2217=VERTEX_POINT('',#7758);
#2218=VERTEX_POINT('',#7760);
#2219=VERTEX_POINT('',#7767);
#2220=VERTEX_POINT('',#7770);
#2221=VERTEX_POINT('',#7771);
#2222=VERTEX_POINT('',#7773);
#2223=VERTEX_POINT('',#7775);
#2224=VERTEX_POINT('',#7778);
#2225=VERTEX_POINT('',#7779);
#2226=VERTEX_POINT('',#7781);
#2227=VERTEX_POINT('',#7783);
#2228=VERTEX_POINT('',#7786);
#2229=VERTEX_POINT('',#7787);
#2230=VERTEX_POINT('',#7789);
#2231=VERTEX_POINT('',#7791);
#2232=VERTEX_POINT('',#7794);
#2233=VERTEX_POINT('',#7795);
#2234=VERTEX_POINT('',#7797);
#2235=VERTEX_POINT('',#7799);
#2236=VERTEX_POINT('',#7802);
#2237=VERTEX_POINT('',#7803);
#2238=VERTEX_POINT('',#7805);
#2239=VERTEX_POINT('',#7807);
#2240=VERTEX_POINT('',#7810);
#2241=VERTEX_POINT('',#7811);
#2242=VERTEX_POINT('',#7813);
#2243=VERTEX_POINT('',#7815);
#2244=VERTEX_POINT('',#7818);
#2245=VERTEX_POINT('',#7819);
#2246=VERTEX_POINT('',#7821);
#2247=VERTEX_POINT('',#7823);
#2248=VERTEX_POINT('',#7826);
#2249=VERTEX_POINT('',#7827);
#2250=VERTEX_POINT('',#7829);
#2251=VERTEX_POINT('',#7831);
#2252=VERTEX_POINT('',#7835);
#2253=VERTEX_POINT('',#7836);
#2254=VERTEX_POINT('',#7838);
#2255=VERTEX_POINT('',#7842);
#2256=VERTEX_POINT('',#7843);
#2257=VERTEX_POINT('',#7845);
#2258=VERTEX_POINT('',#7849);
#2259=VERTEX_POINT('',#7850);
#2260=VERTEX_POINT('',#7852);
#2261=VERTEX_POINT('',#7856);
#2262=VERTEX_POINT('',#7857);
#2263=VERTEX_POINT('',#7859);
#2264=VERTEX_POINT('',#7861);
#2265=VERTEX_POINT('',#7865);
#2266=VERTEX_POINT('',#7866);
#2267=VERTEX_POINT('',#7868);
#2268=VERTEX_POINT('',#7870);
#2269=VERTEX_POINT('',#7874);
#2270=VERTEX_POINT('',#7875);
#2271=VERTEX_POINT('',#7877);
#2272=VERTEX_POINT('',#7879);
#2273=VERTEX_POINT('',#7883);
#2274=VERTEX_POINT('',#7884);
#2275=VERTEX_POINT('',#7886);
#2276=VERTEX_POINT('',#7890);
#2277=VERTEX_POINT('',#7891);
#2278=VERTEX_POINT('',#7893);
#2279=VERTEX_POINT('',#7897);
#2280=VERTEX_POINT('',#7898);
#2281=VERTEX_POINT('',#7900);
#2282=VERTEX_POINT('',#7902);
#2283=VERTEX_POINT('',#7909);
#2284=VERTEX_POINT('',#7911);
#2285=VERTEX_POINT('',#7918);
#2286=VERTEX_POINT('',#7919);
#2287=VERTEX_POINT('',#7921);
#2288=VERTEX_POINT('',#7924);
#2289=VERTEX_POINT('',#7926);
#2290=VERTEX_POINT('',#7929);
#2291=VERTEX_POINT('',#7931);
#2292=VERTEX_POINT('',#7934);
#2293=VERTEX_POINT('',#7936);
#2294=VERTEX_POINT('',#7939);
#2295=VERTEX_POINT('',#7941);
#2296=VERTEX_POINT('',#7943);
#2297=VERTEX_POINT('',#7947);
#2298=VERTEX_POINT('',#7949);
#2299=VERTEX_POINT('',#7953);
#2300=VERTEX_POINT('',#7954);
#2301=VERTEX_POINT('',#7960);
#2302=VERTEX_POINT('',#7963);
#2303=VERTEX_POINT('',#7965);
#2304=VERTEX_POINT('',#7968);
#2305=VERTEX_POINT('',#7970);
#2306=VERTEX_POINT('',#7972);
#2307=VERTEX_POINT('',#7978);
#2308=VERTEX_POINT('',#7980);
#2309=VERTEX_POINT('',#7982);
#2310=VERTEX_POINT('',#7984);
#2311=VERTEX_POINT('',#7986);
#2312=VERTEX_POINT('',#7989);
#2313=VERTEX_POINT('',#7992);
#2314=VERTEX_POINT('',#7994);
#2315=VERTEX_POINT('',#7996);
#2316=VERTEX_POINT('',#8000);
#2317=VERTEX_POINT('',#8002);
#2318=VERTEX_POINT('',#8004);
#2319=VERTEX_POINT('',#8006);
#2320=VERTEX_POINT('',#8008);
#2321=VERTEX_POINT('',#8029);
#2322=VERTEX_POINT('',#8041);
#2323=VERTEX_POINT('',#8042);
#2324=VERTEX_POINT('',#8044);
#2325=VERTEX_POINT('',#8048);
#2326=VERTEX_POINT('',#8050);
#2327=VERTEX_POINT('',#8054);
#2328=VERTEX_POINT('',#8072);
#2329=VERTEX_POINT('',#8073);
#2330=VERTEX_POINT('',#8075);
#2331=VERTEX_POINT('',#8077);
#2332=VERTEX_POINT('',#8080);
#2333=VERTEX_POINT('',#8081);
#2334=VERTEX_POINT('',#8083);
#2335=VERTEX_POINT('',#8085);
#2336=VERTEX_POINT('',#8088);
#2337=VERTEX_POINT('',#8089);
#2338=VERTEX_POINT('',#8091);
#2339=VERTEX_POINT('',#8093);
#2340=VERTEX_POINT('',#8096);
#2341=VERTEX_POINT('',#8097);
#2342=VERTEX_POINT('',#8099);
#2343=VERTEX_POINT('',#8101);
#2344=VERTEX_POINT('',#8104);
#2345=VERTEX_POINT('',#8105);
#2346=VERTEX_POINT('',#8107);
#2347=VERTEX_POINT('',#8109);
#2348=VERTEX_POINT('',#8112);
#2349=VERTEX_POINT('',#8113);
#2350=VERTEX_POINT('',#8115);
#2351=VERTEX_POINT('',#8117);
#2352=VERTEX_POINT('',#8120);
#2353=VERTEX_POINT('',#8121);
#2354=VERTEX_POINT('',#8123);
#2355=VERTEX_POINT('',#8125);
#2356=VERTEX_POINT('',#8128);
#2357=VERTEX_POINT('',#8129);
#2358=VERTEX_POINT('',#8131);
#2359=VERTEX_POINT('',#8133);
#2360=VERTEX_POINT('',#8137);
#2361=VERTEX_POINT('',#8144);
#2362=VERTEX_POINT('',#8151);
#2363=VERTEX_POINT('',#8155);
#2364=VERTEX_POINT('',#8159);
#2365=VERTEX_POINT('',#8166);
#2366=VERTEX_POINT('',#8170);
#2367=VERTEX_POINT('',#8177);
#2368=VERTEX_POINT('',#8181);
#2369=VERTEX_POINT('',#8188);
#2370=VERTEX_POINT('',#8192);
#2371=VERTEX_POINT('',#8199);
#2372=VERTEX_POINT('',#8206);
#2373=VERTEX_POINT('',#8210);
#2374=VERTEX_POINT('',#8217);
#2375=VERTEX_POINT('',#8221);
#2376=VERTEX_POINT('',#8249);
#2377=VERTEX_POINT('',#8250);
#2378=VERTEX_POINT('',#8252);
#2379=VERTEX_POINT('',#8256);
#2380=VERTEX_POINT('',#8258);
#2381=VERTEX_POINT('',#8262);
#2382=VERTEX_POINT('',#8266);
#2383=VERTEX_POINT('',#8268);
#2384=VERTEX_POINT('',#8272);
#2385=VERTEX_POINT('',#8278);
#2386=VERTEX_POINT('',#8279);
#2387=VERTEX_POINT('',#8281);
#2388=VERTEX_POINT('',#8288);
#2389=VERTEX_POINT('',#8289);
#2390=VERTEX_POINT('',#8291);
#2391=VERTEX_POINT('',#8295);
#2392=VERTEX_POINT('',#8297);
#2393=VERTEX_POINT('',#8301);
#2394=VERTEX_POINT('',#8317);
#2395=VERTEX_POINT('',#8318);
#2396=VERTEX_POINT('',#8320);
#2397=VERTEX_POINT('',#8322);
#2398=VERTEX_POINT('',#8325);
#2399=VERTEX_POINT('',#8326);
#2400=VERTEX_POINT('',#8328);
#2401=VERTEX_POINT('',#8330);
#2402=VERTEX_POINT('',#8333);
#2403=VERTEX_POINT('',#8334);
#2404=VERTEX_POINT('',#8336);
#2405=VERTEX_POINT('',#8338);
#2406=VERTEX_POINT('',#8341);
#2407=VERTEX_POINT('',#8342);
#2408=VERTEX_POINT('',#8344);
#2409=VERTEX_POINT('',#8346);
#2410=VERTEX_POINT('',#8349);
#2411=VERTEX_POINT('',#8350);
#2412=VERTEX_POINT('',#8352);
#2413=VERTEX_POINT('',#8354);
#2414=VERTEX_POINT('',#8357);
#2415=VERTEX_POINT('',#8358);
#2416=VERTEX_POINT('',#8360);
#2417=VERTEX_POINT('',#8362);
#2418=VERTEX_POINT('',#8365);
#2419=VERTEX_POINT('',#8366);
#2420=VERTEX_POINT('',#8368);
#2421=VERTEX_POINT('',#8370);
#2422=VERTEX_POINT('',#8373);
#2423=VERTEX_POINT('',#8374);
#2424=VERTEX_POINT('',#8376);
#2425=VERTEX_POINT('',#8378);
#2426=VERTEX_POINT('',#8385);
#2427=VERTEX_POINT('',#8387);
#2428=VERTEX_POINT('',#8391);
#2429=VERTEX_POINT('',#8392);
#2430=VERTEX_POINT('',#8400);
#2431=VERTEX_POINT('',#8401);
#2432=VERTEX_POINT('',#8403);
#2433=VERTEX_POINT('',#8405);
#2434=VERTEX_POINT('',#8421);
#2435=VERTEX_POINT('',#8423);
#2436=VERTEX_POINT('',#8427);
#2437=VERTEX_POINT('',#8428);
#2438=VERTEX_POINT('',#8436);
#2439=VERTEX_POINT('',#8437);
#2440=VERTEX_POINT('',#8439);
#2441=VERTEX_POINT('',#8441);
#2442=VERTEX_POINT('',#8454);
#2443=VERTEX_POINT('',#8455);
#2444=VERTEX_POINT('',#8457);
#2445=VERTEX_POINT('',#8459);
#2446=VERTEX_POINT('',#8472);
#2447=VERTEX_POINT('',#8473);
#2448=VERTEX_POINT('',#8475);
#2449=VERTEX_POINT('',#8477);
#2450=VERTEX_POINT('',#8490);
#2451=VERTEX_POINT('',#8491);
#2452=VERTEX_POINT('',#8493);
#2453=VERTEX_POINT('',#8495);
#2454=VERTEX_POINT('',#8511);
#2455=VERTEX_POINT('',#8513);
#2456=VERTEX_POINT('',#8517);
#2457=VERTEX_POINT('',#8518);
#2458=VERTEX_POINT('',#8544);
#2459=VERTEX_POINT('',#8545);
#2460=VERTEX_POINT('',#8547);
#2461=VERTEX_POINT('',#8549);
#2462=VERTEX_POINT('',#8551);
#2463=VERTEX_POINT('',#8553);
#2464=VERTEX_POINT('',#8555);
#2465=VERTEX_POINT('',#8557);
#2466=VERTEX_POINT('',#8559);
#2467=VERTEX_POINT('',#8561);
#2468=VERTEX_POINT('',#8563);
#2469=VERTEX_POINT('',#8565);
#2470=VERTEX_POINT('',#8567);
#2471=VERTEX_POINT('',#8569);
#2472=VERTEX_POINT('',#8573);
#2473=VERTEX_POINT('',#8574);
#2474=VERTEX_POINT('',#8579);
#2475=VERTEX_POINT('',#8581);
#2476=VERTEX_POINT('',#8585);
#2477=VERTEX_POINT('',#8587);
#2478=VERTEX_POINT('',#8590);
#2479=VERTEX_POINT('',#8592);
#2480=VERTEX_POINT('',#8595);
#2481=VERTEX_POINT('',#8597);
#2482=VERTEX_POINT('',#8601);
#2483=VERTEX_POINT('',#8603);
#2484=VERTEX_POINT('',#8607);
#2485=VERTEX_POINT('',#8609);
#2486=VERTEX_POINT('',#8613);
#2487=VERTEX_POINT('',#8615);
#2488=VERTEX_POINT('',#8619);
#2489=VERTEX_POINT('',#8620);
#2490=VERTEX_POINT('',#8622);
#2491=VERTEX_POINT('',#8629);
#2492=VERTEX_POINT('',#8639);
#2493=VERTEX_POINT('',#8641);
#2494=VERTEX_POINT('',#8644);
#2495=VERTEX_POINT('',#8646);
#2496=VERTEX_POINT('',#8648);
#2497=VERTEX_POINT('',#8652);
#2498=VERTEX_POINT('',#8686);
#2499=VERTEX_POINT('',#8687);
#2500=VERTEX_POINT('',#8689);
#2501=VERTEX_POINT('',#8691);
#2502=VERTEX_POINT('',#8696);
#2503=VERTEX_POINT('',#8699);
#2504=VERTEX_POINT('',#8708);
#2505=VERTEX_POINT('',#8710);
#2506=VERTEX_POINT('',#8713);
#2507=VERTEX_POINT('',#8717);
#2508=VERTEX_POINT('',#8723);
#2509=VERTEX_POINT('',#8724);
#2510=VERTEX_POINT('',#8726);
#2511=VERTEX_POINT('',#8731);
#2512=VERTEX_POINT('',#8734);
#2513=VERTEX_POINT('',#8738);
#2514=VERTEX_POINT('',#8739);
#2515=VERTEX_POINT('',#8744);
#2516=VERTEX_POINT('',#8748);
#2517=VERTEX_POINT('',#8749);
#2518=VERTEX_POINT('',#8751);
#2519=VERTEX_POINT('',#8756);
#2520=VERTEX_POINT('',#8759);
#2521=VERTEX_POINT('',#8763);
#2522=VERTEX_POINT('',#8764);
#2523=VERTEX_POINT('',#8769);
#2524=VERTEX_POINT('',#8773);
#2525=VERTEX_POINT('',#8776);
#2526=VERTEX_POINT('',#8780);
#2527=VERTEX_POINT('',#8783);
#2528=VERTEX_POINT('',#8787);
#2529=VERTEX_POINT('',#8791);
#2530=VERTEX_POINT('',#8795);
#2531=VERTEX_POINT('',#8799);
#2532=VERTEX_POINT('',#8803);
#2533=VERTEX_POINT('',#8806);
#2534=VERTEX_POINT('',#8811);
#2535=VERTEX_POINT('',#8814);
#2536=VERTEX_POINT('',#8818);
#2537=VERTEX_POINT('',#8821);
#2538=VERTEX_POINT('',#8825);
#2539=VERTEX_POINT('',#8828);
#2540=VERTEX_POINT('',#8834);
#2541=VERTEX_POINT('',#8836);
#2542=VERTEX_POINT('',#8839);
#2543=VERTEX_POINT('',#8843);
#2544=VERTEX_POINT('',#8846);
#2545=VERTEX_POINT('',#8850);
#2546=VERTEX_POINT('',#8854);
#2547=VERTEX_POINT('',#8860);
#2548=VERTEX_POINT('',#8862);
#2549=VERTEX_POINT('',#8865);
#2550=VERTEX_POINT('',#8869);
#2551=VERTEX_POINT('',#8875);
#2552=VERTEX_POINT('',#8877);
#2553=VERTEX_POINT('',#8880);
#2554=VERTEX_POINT('',#8884);
#2555=VERTEX_POINT('',#8887);
#2556=VERTEX_POINT('',#8891);
#2557=VERTEX_POINT('',#8895);
#2558=EDGE_CURVE('',#2082,#2083,#1172,.T.);
#2559=EDGE_CURVE('',#2083,#2084,#916,.T.);
#2560=EDGE_CURVE('',#2084,#2085,#1173,.T.);
#2561=EDGE_CURVE('',#2085,#2086,#917,.T.);
#2562=EDGE_CURVE('',#2086,#2087,#1174,.T.);
#2563=EDGE_CURVE('',#2087,#2088,#918,.T.);
#2564=EDGE_CURVE('',#2088,#2089,#1175,.T.);
#2565=EDGE_CURVE('',#2089,#2090,#919,.T.);
#2566=EDGE_CURVE('',#2090,#2091,#1176,.T.);
#2567=EDGE_CURVE('',#2091,#2092,#920,.T.);
#2568=EDGE_CURVE('',#2092,#2093,#921,.T.);
#2569=EDGE_CURVE('',#2093,#2094,#1177,.T.);
#2570=EDGE_CURVE('',#2094,#2095,#922,.T.);
#2571=EDGE_CURVE('',#2095,#2082,#923,.T.);
#2572=EDGE_CURVE('',#2096,#2097,#1178,.T.);
#2573=EDGE_CURVE('',#2096,#2091,#1179,.F.);
#2574=EDGE_CURVE('',#2090,#2097,#1180,.T.);
#2575=EDGE_CURVE('',#2084,#2098,#1181,.T.);
#2576=EDGE_CURVE('',#2099,#2098,#1182,.T.);
#2577=EDGE_CURVE('',#2099,#2085,#1183,.T.);
#2578=EDGE_CURVE('',#2086,#2100,#1184,.T.);
#2579=EDGE_CURVE('',#2100,#2101,#1185,.T.);
#2580=EDGE_CURVE('',#2101,#2087,#1186,.T.);
#2581=EDGE_CURVE('',#2102,#2102,#924,.T.);
#2582=EDGE_CURVE('',#2103,#2103,#925,.T.);
#2583=EDGE_CURVE('',#2088,#2104,#1187,.T.);
#2584=EDGE_CURVE('',#2104,#2105,#1188,.T.);
#2585=EDGE_CURVE('',#2105,#2089,#1189,.T.);
#2586=EDGE_CURVE('',#2106,#2106,#926,.T.);
#2587=EDGE_CURVE('',#2106,#2107,#1190,.T.);
#2588=EDGE_CURVE('',#2107,#2107,#927,.T.);
#2589=EDGE_CURVE('',#2082,#2108,#1191,.T.);
#2590=EDGE_CURVE('',#2109,#2108,#1192,.T.);
#2591=EDGE_CURVE('',#2109,#2083,#1193,.T.);
#2592=EDGE_CURVE('',#2110,#2110,#928,.T.);
#2593=EDGE_CURVE('',#2110,#2111,#1194,.T.);
#2594=EDGE_CURVE('',#2111,#2111,#929,.T.);
#2595=EDGE_CURVE('',#2112,#2113,#1195,.T.);
#2596=EDGE_CURVE('',#2113,#2114,#930,.F.);
#2597=EDGE_CURVE('',#2114,#2096,#931,.T.);
#2598=EDGE_CURVE('',#2097,#2105,#932,.F.);
#2599=EDGE_CURVE('',#2104,#2101,#933,.F.);
#2600=EDGE_CURVE('',#2100,#2099,#934,.F.);
#2601=EDGE_CURVE('',#2098,#2109,#935,.F.);
#2602=EDGE_CURVE('',#2108,#2115,#936,.T.);
#2603=EDGE_CURVE('',#2115,#2112,#937,.F.);
#2604=EDGE_CURVE('',#2116,#2093,#1196,.T.);
#2605=EDGE_CURVE('',#2117,#2116,#938,.T.);
#2606=EDGE_CURVE('',#2118,#2117,#939,.T.);
#2607=EDGE_CURVE('',#2118,#2113,#1197,.T.);
#2608=EDGE_CURVE('',#2112,#2119,#1198,.F.);
#2609=EDGE_CURVE('',#2120,#2119,#940,.T.);
#2610=EDGE_CURVE('',#2120,#2094,#1199,.T.);
#2611=EDGE_CURVE('',#2103,#2121,#1200,.T.);
#2612=EDGE_CURVE('',#2121,#2120,#147,.F.);
#2613=EDGE_CURVE('',#2119,#2121,#148,.F.);
#2614=EDGE_CURVE('',#2102,#2117,#1201,.T.);
#2615=EDGE_CURVE('',#2116,#2118,#149,.T.);
#2616=EDGE_CURVE('',#2114,#2092,#1202,.T.);
#2617=EDGE_CURVE('',#2115,#2095,#1203,.T.);
#2618=EDGE_CURVE('',#2122,#2123,#1204,.T.);
#2619=EDGE_CURVE('',#2124,#2122,#1205,.T.);
#2620=EDGE_CURVE('',#2125,#2124,#1206,.T.);
#2621=EDGE_CURVE('',#2123,#2125,#1207,.T.);
#2622=EDGE_CURVE('',#2126,#2127,#1208,.T.);
#2623=EDGE_CURVE('',#2128,#2126,#1209,.T.);
#2624=EDGE_CURVE('',#2129,#2128,#1210,.T.);
#2625=EDGE_CURVE('',#2129,#2127,#1211,.T.);
#2626=EDGE_CURVE('',#2127,#2122,#1212,.T.);
#2627=EDGE_CURVE('',#2124,#2129,#1213,.T.);
#2628=EDGE_CURVE('',#2125,#2130,#1214,.T.);
#2629=EDGE_CURVE('',#2131,#2130,#1215,.T.);
#2630=EDGE_CURVE('',#2132,#2131,#1216,.T.);
#2631=EDGE_CURVE('',#2133,#2132,#1217,.T.);
#2632=EDGE_CURVE('',#2133,#2134,#1218,.T.);
#2633=EDGE_CURVE('',#2134,#2135,#1219,.T.);
#2634=EDGE_CURVE('',#2123,#2135,#1220,.T.);
#2635=EDGE_CURVE('',#2136,#2126,#1221,.T.);
#2636=EDGE_CURVE('',#2137,#2136,#1222,.T.);
#2637=EDGE_CURVE('',#2137,#2138,#1223,.T.);
#2638=EDGE_CURVE('',#2138,#2139,#1224,.T.);
#2639=EDGE_CURVE('',#2140,#2139,#1225,.T.);
#2640=EDGE_CURVE('',#2140,#2141,#1226,.T.);
#2641=EDGE_CURVE('',#2141,#2128,#1227,.T.);
#2642=EDGE_CURVE('',#2142,#2135,#1228,.T.);
#2643=EDGE_CURVE('',#2143,#2142,#1229,.T.);
#2644=EDGE_CURVE('',#2143,#2136,#1230,.T.);
#2645=EDGE_CURVE('',#2144,#2145,#1231,.T.);
#2646=EDGE_CURVE('',#2146,#2145,#1232,.T.);
#2647=EDGE_CURVE('',#2147,#2146,#1233,.T.);
#2648=EDGE_CURVE('',#2144,#2147,#1234,.T.);
#2649=EDGE_CURVE('',#2148,#2145,#1235,.T.);
#2650=EDGE_CURVE('',#2149,#2148,#1236,.T.);
#2651=EDGE_CURVE('',#2149,#2146,#1237,.T.);
#2652=EDGE_CURVE('',#2150,#2151,#1238,.T.);
#2653=EDGE_CURVE('',#2151,#2149,#1239,.T.);
#2654=EDGE_CURVE('',#2148,#2150,#1240,.T.);
#2655=EDGE_CURVE('',#2137,#2152,#1241,.T.);
#2656=EDGE_CURVE('',#2152,#2143,#1242,.T.);
#2657=EDGE_CURVE('',#2153,#2154,#1243,.T.);
#2658=EDGE_CURVE('',#2153,#2155,#1244,.F.);
#2659=EDGE_CURVE('',#2155,#2156,#1245,.T.);
#2660=EDGE_CURVE('',#2156,#2154,#1246,.T.);
#2661=EDGE_CURVE('',#2157,#2158,#1247,.T.);
#2662=EDGE_CURVE('',#2157,#2159,#1248,.F.);
#2663=EDGE_CURVE('',#2159,#2160,#1249,.T.);
#2664=EDGE_CURVE('',#2160,#2158,#1250,.T.);
#2665=EDGE_CURVE('',#2161,#2162,#1251,.T.);
#2666=EDGE_CURVE('',#2163,#2162,#1252,.T.);
#2667=EDGE_CURVE('',#2164,#2163,#1253,.T.);
#2668=EDGE_CURVE('',#2164,#2161,#1254,.T.);
#2669=EDGE_CURVE('',#2165,#2166,#1255,.T.);
#2670=EDGE_CURVE('',#2167,#2166,#1256,.T.);
#2671=EDGE_CURVE('',#2168,#2167,#1257,.T.);
#2672=EDGE_CURVE('',#2168,#2165,#1258,.T.);
#2673=EDGE_CURVE('',#2169,#2170,#1259,.T.);
#2674=EDGE_CURVE('',#2171,#2170,#1260,.T.);
#2675=EDGE_CURVE('',#2172,#2171,#1261,.T.);
#2676=EDGE_CURVE('',#2172,#2169,#1262,.T.);
#2677=EDGE_CURVE('',#2173,#2174,#1263,.T.);
#2678=EDGE_CURVE('',#2173,#2175,#1264,.F.);
#2679=EDGE_CURVE('',#2175,#2176,#1265,.T.);
#2680=EDGE_CURVE('',#2176,#2174,#1266,.T.);
#2681=EDGE_CURVE('',#2177,#2178,#1267,.T.);
#2682=EDGE_CURVE('',#2179,#2178,#1268,.T.);
#2683=EDGE_CURVE('',#2180,#2179,#1269,.T.);
#2684=EDGE_CURVE('',#2180,#2177,#1270,.T.);
#2685=EDGE_CURVE('',#2181,#2182,#1271,.T.);
#2686=EDGE_CURVE('',#2183,#2182,#1272,.T.);
#2687=EDGE_CURVE('',#2184,#2183,#1273,.T.);
#2688=EDGE_CURVE('',#2184,#2181,#1274,.T.);
#2689=EDGE_CURVE('',#2185,#2186,#941,.T.);
#2690=EDGE_CURVE('',#2185,#2187,#1275,.T.);
#2691=EDGE_CURVE('',#2187,#2186,#1276,.T.);
#2692=EDGE_CURVE('',#2188,#2189,#1277,.T.);
#2693=EDGE_CURVE('',#2188,#2190,#942,.T.);
#2694=EDGE_CURVE('',#2189,#2190,#1278,.T.);
#2695=EDGE_CURVE('',#2191,#2192,#943,.T.);
#2696=EDGE_CURVE('',#2191,#2193,#1279,.T.);
#2697=EDGE_CURVE('',#2193,#2192,#1280,.T.);
#2698=EDGE_CURVE('',#2194,#2195,#1281,.T.);
#2699=EDGE_CURVE('',#2194,#2196,#944,.T.);
#2700=EDGE_CURVE('',#2195,#2196,#1282,.T.);
#2701=EDGE_CURVE('',#2197,#2198,#945,.T.);
#2702=EDGE_CURVE('',#2199,#2197,#1283,.T.);
#2703=EDGE_CURVE('',#2199,#2198,#1284,.T.);
#2704=EDGE_CURVE('',#2200,#2201,#946,.T.);
#2705=EDGE_CURVE('',#2202,#2200,#1285,.T.);
#2706=EDGE_CURVE('',#2202,#2201,#1286,.T.);
#2707=EDGE_CURVE('',#2200,#2203,#1287,.T.);
#2708=EDGE_CURVE('',#2204,#2203,#1288,.T.);
#2709=EDGE_CURVE('',#2202,#2204,#1289,.T.);
#2710=EDGE_CURVE('',#2205,#2206,#1290,.T.);
#2711=EDGE_CURVE('',#2206,#2207,#947,.T.);
#2712=EDGE_CURVE('',#2205,#2207,#1291,.T.);
#2713=EDGE_CURVE('',#2208,#2209,#948,.T.);
#2714=EDGE_CURVE('',#2208,#2210,#1292,.T.);
#2715=EDGE_CURVE('',#2210,#2209,#1293,.T.);
#2716=EDGE_CURVE('',#2211,#2212,#1294,.T.);
#2717=EDGE_CURVE('',#2211,#2213,#949,.T.);
#2718=EDGE_CURVE('',#2212,#2213,#1295,.T.);
#2719=EDGE_CURVE('',#2214,#2215,#1296,.T.);
#2720=EDGE_CURVE('',#2214,#2188,#1297,.T.);
#2721=EDGE_CURVE('',#2187,#2189,#1298,.T.);
#2722=EDGE_CURVE('',#2185,#2194,#1299,.T.);
#2723=EDGE_CURVE('',#2193,#2195,#1300,.T.);
#2724=EDGE_CURVE('',#2191,#2201,#1301,.T.);
#2725=EDGE_CURVE('',#2204,#2216,#1302,.T.);
#2726=EDGE_CURVE('',#2216,#2211,#1303,.T.);
#2727=EDGE_CURVE('',#2210,#2212,#1304,.T.);
#2728=EDGE_CURVE('',#2217,#2208,#1305,.F.);
#2729=EDGE_CURVE('',#2217,#2218,#1306,.T.);
#2730=EDGE_CURVE('',#2218,#2215,#1307,.T.);
#2731=EDGE_CURVE('',#2140,#2144,#1308,.T.);
#2732=EDGE_CURVE('',#2141,#2147,#1309,.T.);
#2733=EDGE_CURVE('',#2134,#2219,#1310,.T.);
#2734=EDGE_CURVE('',#2219,#2142,#1311,.T.);
#2735=EDGE_CURVE('',#2220,#2221,#1312,.T.);
#2736=EDGE_CURVE('',#2220,#2222,#1313,.F.);
#2737=EDGE_CURVE('',#2222,#2223,#1314,.T.);
#2738=EDGE_CURVE('',#2223,#2221,#1315,.T.);
#2739=EDGE_CURVE('',#2224,#2225,#1316,.T.);
#2740=EDGE_CURVE('',#2226,#2225,#1317,.T.);
#2741=EDGE_CURVE('',#2227,#2226,#1318,.T.);
#2742=EDGE_CURVE('',#2227,#2224,#1319,.T.);
#2743=EDGE_CURVE('',#2228,#2229,#1320,.T.);
#2744=EDGE_CURVE('',#2228,#2230,#1321,.F.);
#2745=EDGE_CURVE('',#2230,#2231,#1322,.T.);
#2746=EDGE_CURVE('',#2231,#2229,#1323,.T.);
#2747=EDGE_CURVE('',#2232,#2233,#1324,.T.);
#2748=EDGE_CURVE('',#2234,#2233,#1325,.T.);
#2749=EDGE_CURVE('',#2235,#2234,#1326,.T.);
#2750=EDGE_CURVE('',#2235,#2232,#1327,.T.);
#2751=EDGE_CURVE('',#2236,#2237,#1328,.T.);
#2752=EDGE_CURVE('',#2238,#2237,#1329,.T.);
#2753=EDGE_CURVE('',#2239,#2238,#1330,.T.);
#2754=EDGE_CURVE('',#2239,#2236,#1331,.T.);
#2755=EDGE_CURVE('',#2240,#2241,#1332,.T.);
#2756=EDGE_CURVE('',#2240,#2242,#1333,.F.);
#2757=EDGE_CURVE('',#2242,#2243,#1334,.T.);
#2758=EDGE_CURVE('',#2243,#2241,#1335,.T.);
#2759=EDGE_CURVE('',#2244,#2245,#1336,.T.);
#2760=EDGE_CURVE('',#2244,#2246,#1337,.F.);
#2761=EDGE_CURVE('',#2246,#2247,#1338,.T.);
#2762=EDGE_CURVE('',#2247,#2245,#1339,.T.);
#2763=EDGE_CURVE('',#2248,#2249,#1340,.T.);
#2764=EDGE_CURVE('',#2248,#2250,#1341,.F.);
#2765=EDGE_CURVE('',#2250,#2251,#1342,.T.);
#2766=EDGE_CURVE('',#2251,#2249,#1343,.T.);
#2767=EDGE_CURVE('',#2252,#2253,#950,.T.);
#2768=EDGE_CURVE('',#2252,#2254,#1344,.T.);
#2769=EDGE_CURVE('',#2254,#2253,#1345,.T.);
#2770=EDGE_CURVE('',#2255,#2256,#1346,.T.);
#2771=EDGE_CURVE('',#2255,#2257,#951,.T.);
#2772=EDGE_CURVE('',#2256,#2257,#1347,.T.);
#2773=EDGE_CURVE('',#2258,#2259,#1348,.T.);
#2774=EDGE_CURVE('',#2258,#2260,#952,.T.);
#2775=EDGE_CURVE('',#2259,#2260,#1349,.T.);
#2776=EDGE_CURVE('',#2261,#2262,#1350,.T.);
#2777=EDGE_CURVE('',#2262,#2263,#1351,.T.);
#2778=EDGE_CURVE('',#2264,#2263,#1352,.T.);
#2779=EDGE_CURVE('',#2261,#2264,#1353,.T.);
#2780=EDGE_CURVE('',#2265,#2266,#1354,.T.);
#2781=EDGE_CURVE('',#2266,#2267,#1355,.T.);
#2782=EDGE_CURVE('',#2268,#2267,#1356,.T.);
#2783=EDGE_CURVE('',#2265,#2268,#1357,.T.);
#2784=EDGE_CURVE('',#2269,#2270,#1358,.T.);
#2785=EDGE_CURVE('',#2270,#2271,#1359,.T.);
#2786=EDGE_CURVE('',#2272,#2271,#1360,.T.);
#2787=EDGE_CURVE('',#2269,#2272,#1361,.T.);
#2788=EDGE_CURVE('',#2273,#2274,#953,.T.);
#2789=EDGE_CURVE('',#2273,#2275,#1362,.T.);
#2790=EDGE_CURVE('',#2275,#2274,#1363,.T.);
#2791=EDGE_CURVE('',#2276,#2277,#1364,.T.);
#2792=EDGE_CURVE('',#2276,#2278,#954,.T.);
#2793=EDGE_CURVE('',#2277,#2278,#1365,.T.);
#2794=EDGE_CURVE('',#2279,#2280,#1366,.T.);
#2795=EDGE_CURVE('',#2280,#2281,#1367,.T.);
#2796=EDGE_CURVE('',#2282,#2281,#1368,.T.);
#2797=EDGE_CURVE('',#2279,#2282,#1369,.T.);
#2798=EDGE_CURVE('',#2253,#2257,#1370,.T.);
#2799=EDGE_CURVE('',#2254,#2256,#1371,.T.);
#2800=EDGE_CURVE('',#2283,#2260,#1372,.T.);
#2801=EDGE_CURVE('',#2284,#2283,#1373,.T.);
#2802=EDGE_CURVE('',#2284,#2259,#1374,.T.);
#2803=EDGE_CURVE('',#2274,#2278,#1375,.T.);
#2804=EDGE_CURVE('',#2275,#2277,#1376,.T.);
#2805=EDGE_CURVE('',#2285,#2286,#1377,.T.);
#2806=EDGE_CURVE('',#2285,#2287,#1378,.T.);
#2807=EDGE_CURVE('',#2279,#2287,#1379,.T.);
#2808=EDGE_CURVE('',#2282,#2288,#1380,.T.);
#2809=EDGE_CURVE('',#2288,#2289,#1381,.T.);
#2810=EDGE_CURVE('',#2269,#2289,#1382,.T.);
#2811=EDGE_CURVE('',#2272,#2290,#1383,.T.);
#2812=EDGE_CURVE('',#2290,#2291,#1384,.T.);
#2813=EDGE_CURVE('',#2265,#2291,#1385,.T.);
#2814=EDGE_CURVE('',#2268,#2292,#1386,.T.);
#2815=EDGE_CURVE('',#2292,#2293,#1387,.T.);
#2816=EDGE_CURVE('',#2261,#2293,#1388,.T.);
#2817=EDGE_CURVE('',#2264,#2294,#1389,.T.);
#2818=EDGE_CURVE('',#2295,#2294,#1390,.F.);
#2819=EDGE_CURVE('',#2295,#2296,#1391,.T.);
#2820=EDGE_CURVE('',#2286,#2296,#1392,.T.);
#2821=EDGE_CURVE('',#2130,#2297,#1393,.T.);
#2822=EDGE_CURVE('',#2297,#2298,#1394,.F.);
#2823=EDGE_CURVE('',#2131,#2298,#1395,.T.);
#2824=EDGE_CURVE('',#2299,#2300,#1396,.T.);
#2825=EDGE_CURVE('',#2299,#2138,#1397,.T.);
#2826=EDGE_CURVE('',#2152,#2219,#1398,.T.);
#2827=EDGE_CURVE('',#2300,#2133,#1399,.T.);
#2828=EDGE_CURVE('',#2301,#2217,#955,.T.);
#2829=EDGE_CURVE('',#2150,#2301,#1400,.T.);
#2830=EDGE_CURVE('',#2139,#2302,#1401,.T.);
#2831=EDGE_CURVE('',#2303,#2302,#1402,.T.);
#2832=EDGE_CURVE('',#2132,#2303,#1403,.T.);
#2833=EDGE_CURVE('',#2298,#2304,#956,.T.);
#2834=EDGE_CURVE('',#2305,#2304,#1404,.T.);
#2835=EDGE_CURVE('',#2305,#2306,#1405,.T.);
#2836=EDGE_CURVE('',#2306,#2285,#957,.T.);
#2837=EDGE_CURVE('',#2218,#2286,#1406,.T.);
#2838=EDGE_CURVE('',#2215,#2296,#1407,.T.);
#2839=EDGE_CURVE('',#2307,#2307,#958,.T.);
#2840=EDGE_CURVE('',#2308,#2308,#959,.T.);
#2841=EDGE_CURVE('',#2309,#2309,#960,.T.);
#2842=EDGE_CURVE('',#2310,#2310,#961,.T.);
#2843=EDGE_CURVE('',#2311,#2311,#962,.T.);
#2844=EDGE_CURVE('',#2151,#2312,#1408,.T.);
#2845=EDGE_CURVE('',#2214,#2312,#963,.T.);
#2846=EDGE_CURVE('',#2313,#2295,#964,.T.);
#2847=EDGE_CURVE('',#2314,#2313,#1409,.T.);
#2848=EDGE_CURVE('',#2314,#2315,#1410,.T.);
#2849=EDGE_CURVE('',#2315,#2297,#965,.F.);
#2850=EDGE_CURVE('',#2316,#2316,#966,.T.);
#2851=EDGE_CURVE('',#2317,#2317,#967,.T.);
#2852=EDGE_CURVE('',#2318,#2318,#968,.T.);
#2853=EDGE_CURVE('',#2319,#2319,#969,.T.);
#2854=EDGE_CURVE('',#2320,#2320,#970,.T.);
#2855=EDGE_CURVE('',#2299,#2302,#1411,.T.);
#2856=EDGE_CURVE('',#2300,#2303,#1412,.T.);
#2857=EDGE_CURVE('',#2320,#2311,#1413,.T.);
#2858=EDGE_CURVE('',#2319,#2310,#1414,.T.);
#2859=EDGE_CURVE('',#2318,#2309,#1415,.T.);
#2860=EDGE_CURVE('',#2317,#2308,#1416,.T.);
#2861=EDGE_CURVE('',#2316,#2307,#1417,.T.);
#2862=EDGE_CURVE('',#2304,#2315,#1418,.T.);
#2863=EDGE_CURVE('',#2305,#2314,#1419,.T.);
#2864=EDGE_CURVE('',#2321,#2283,#971,.T.);
#2865=EDGE_CURVE('',#2321,#2284,#1420,.T.);
#2866=EDGE_CURVE('',#2262,#2293,#972,.T.);
#2867=EDGE_CURVE('',#2263,#2294,#973,.T.);
#2868=EDGE_CURVE('',#2266,#2291,#974,.T.);
#2869=EDGE_CURVE('',#2267,#2292,#975,.T.);
#2870=EDGE_CURVE('',#2322,#2323,#976,.T.);
#2871=EDGE_CURVE('',#2324,#2322,#1421,.T.);
#2872=EDGE_CURVE('',#2324,#2323,#1422,.T.);
#2873=EDGE_CURVE('',#2322,#2325,#1423,.F.);
#2874=EDGE_CURVE('',#2326,#2325,#1424,.T.);
#2875=EDGE_CURVE('',#2324,#2326,#1425,.T.);
#2876=EDGE_CURVE('',#2325,#2327,#977,.T.);
#2877=EDGE_CURVE('',#2326,#2327,#1426,.T.);
#2878=EDGE_CURVE('',#2270,#2289,#978,.T.);
#2879=EDGE_CURVE('',#2271,#2290,#979,.T.);
#2880=EDGE_CURVE('',#2280,#2287,#980,.T.);
#2881=EDGE_CURVE('',#2281,#2288,#981,.T.);
#2882=EDGE_CURVE('',#2306,#2273,#1427,.T.);
#2883=EDGE_CURVE('',#2255,#2313,#1428,.T.);
#2884=EDGE_CURVE('',#2258,#2252,#1429,.T.);
#2885=EDGE_CURVE('',#2323,#2321,#1430,.T.);
#2886=EDGE_CURVE('',#2276,#2327,#1431,.T.);
#2887=EDGE_CURVE('',#2328,#2329,#982,.T.);
#2888=EDGE_CURVE('',#2329,#2330,#1432,.T.);
#2889=EDGE_CURVE('',#2331,#2330,#983,.T.);
#2890=EDGE_CURVE('',#2331,#2328,#1433,.F.);
#2891=EDGE_CURVE('',#2332,#2333,#984,.T.);
#2892=EDGE_CURVE('',#2333,#2334,#1434,.T.);
#2893=EDGE_CURVE('',#2335,#2334,#985,.T.);
#2894=EDGE_CURVE('',#2335,#2332,#1435,.F.);
#2895=EDGE_CURVE('',#2336,#2337,#1436,.F.);
#2896=EDGE_CURVE('',#2337,#2338,#986,.T.);
#2897=EDGE_CURVE('',#2339,#2338,#1437,.F.);
#2898=EDGE_CURVE('',#2336,#2339,#987,.T.);
#2899=EDGE_CURVE('',#2340,#2341,#1438,.F.);
#2900=EDGE_CURVE('',#2341,#2342,#988,.T.);
#2901=EDGE_CURVE('',#2343,#2342,#1439,.F.);
#2902=EDGE_CURVE('',#2340,#2343,#989,.T.);
#2903=EDGE_CURVE('',#2344,#2345,#1440,.T.);
#2904=EDGE_CURVE('',#2345,#2346,#990,.T.);
#2905=EDGE_CURVE('',#2347,#2346,#1441,.T.);
#2906=EDGE_CURVE('',#2344,#2347,#991,.T.);
#2907=EDGE_CURVE('',#2348,#2349,#1442,.F.);
#2908=EDGE_CURVE('',#2349,#2350,#992,.T.);
#2909=EDGE_CURVE('',#2351,#2350,#1443,.F.);
#2910=EDGE_CURVE('',#2348,#2351,#993,.T.);
#2911=EDGE_CURVE('',#2352,#2353,#994,.T.);
#2912=EDGE_CURVE('',#2353,#2354,#1444,.T.);
#2913=EDGE_CURVE('',#2355,#2354,#995,.T.);
#2914=EDGE_CURVE('',#2355,#2352,#1445,.F.);
#2915=EDGE_CURVE('',#2356,#2357,#1446,.F.);
#2916=EDGE_CURVE('',#2357,#2358,#996,.T.);
#2917=EDGE_CURVE('',#2359,#2358,#1447,.F.);
#2918=EDGE_CURVE('',#2356,#2359,#997,.T.);
#2919=EDGE_CURVE('',#2222,#2360,#998,.T.);
#2920=EDGE_CURVE('',#2360,#2356,#999,.T.);
#2921=EDGE_CURVE('',#2359,#2223,#1448,.T.);
#2922=EDGE_CURVE('',#2358,#2221,#1449,.T.);
#2923=EDGE_CURVE('',#2357,#2361,#1000,.F.);
#2924=EDGE_CURVE('',#2361,#2220,#1001,.F.);
#2925=EDGE_CURVE('',#2355,#2227,#1450,.T.);
#2926=EDGE_CURVE('',#2352,#2226,#1451,.T.);
#2927=EDGE_CURVE('',#2354,#2362,#1002,.T.);
#2928=EDGE_CURVE('',#2362,#2224,#1003,.T.);
#2929=EDGE_CURVE('',#2225,#2363,#1004,.F.);
#2930=EDGE_CURVE('',#2363,#2353,#1005,.F.);
#2931=EDGE_CURVE('',#2250,#2364,#1006,.T.);
#2932=EDGE_CURVE('',#2364,#2348,#1007,.T.);
#2933=EDGE_CURVE('',#2351,#2251,#1452,.T.);
#2934=EDGE_CURVE('',#2350,#2249,#1453,.T.);
#2935=EDGE_CURVE('',#2349,#2365,#1008,.F.);
#2936=EDGE_CURVE('',#2365,#2248,#1009,.F.);
#2937=EDGE_CURVE('',#2230,#2366,#1010,.T.);
#2938=EDGE_CURVE('',#2366,#2344,#1011,.T.);
#2939=EDGE_CURVE('',#2347,#2231,#1454,.T.);
#2940=EDGE_CURVE('',#2346,#2229,#1455,.T.);
#2941=EDGE_CURVE('',#2345,#2367,#1012,.F.);
#2942=EDGE_CURVE('',#2367,#2228,#1013,.F.);
#2943=EDGE_CURVE('',#2246,#2368,#1014,.T.);
#2944=EDGE_CURVE('',#2368,#2340,#1015,.T.);
#2945=EDGE_CURVE('',#2343,#2247,#1456,.T.);
#2946=EDGE_CURVE('',#2342,#2245,#1457,.T.);
#2947=EDGE_CURVE('',#2341,#2369,#1016,.F.);
#2948=EDGE_CURVE('',#2369,#2244,#1017,.F.);
#2949=EDGE_CURVE('',#2242,#2370,#1018,.T.);
#2950=EDGE_CURVE('',#2370,#2336,#1019,.T.);
#2951=EDGE_CURVE('',#2339,#2243,#1458,.T.);
#2952=EDGE_CURVE('',#2338,#2241,#1459,.T.);
#2953=EDGE_CURVE('',#2337,#2371,#1020,.F.);
#2954=EDGE_CURVE('',#2371,#2240,#1021,.F.);
#2955=EDGE_CURVE('',#2335,#2235,#1460,.T.);
#2956=EDGE_CURVE('',#2332,#2234,#1461,.T.);
#2957=EDGE_CURVE('',#2334,#2372,#1022,.T.);
#2958=EDGE_CURVE('',#2372,#2232,#1023,.T.);
#2959=EDGE_CURVE('',#2233,#2373,#1024,.F.);
#2960=EDGE_CURVE('',#2373,#2333,#1025,.F.);
#2961=EDGE_CURVE('',#2331,#2239,#1462,.T.);
#2962=EDGE_CURVE('',#2328,#2238,#1463,.T.);
#2963=EDGE_CURVE('',#2330,#2374,#1026,.T.);
#2964=EDGE_CURVE('',#2374,#2236,#1027,.T.);
#2965=EDGE_CURVE('',#2237,#2375,#1028,.F.);
#2966=EDGE_CURVE('',#2375,#2329,#1029,.F.);
#2967=EDGE_CURVE('',#2365,#2364,#1464,.T.);
#2968=EDGE_CURVE('',#2369,#2368,#1465,.T.);
#2969=EDGE_CURVE('',#2371,#2370,#1466,.T.);
#2970=EDGE_CURVE('',#2374,#2375,#1467,.F.);
#2971=EDGE_CURVE('',#2372,#2373,#1468,.F.);
#2972=EDGE_CURVE('',#2367,#2366,#1469,.F.);
#2973=EDGE_CURVE('',#2362,#2363,#1470,.F.);
#2974=EDGE_CURVE('',#2361,#2360,#1471,.T.);
#2975=EDGE_CURVE('',#2376,#2377,#1030,.T.);
#2976=EDGE_CURVE('',#2378,#2376,#1472,.T.);
#2977=EDGE_CURVE('',#2378,#2377,#1473,.T.);
#2978=EDGE_CURVE('',#2376,#2379,#1474,.F.);
#2979=EDGE_CURVE('',#2380,#2379,#1475,.T.);
#2980=EDGE_CURVE('',#2378,#2380,#1476,.T.);
#2981=EDGE_CURVE('',#2379,#2381,#1031,.T.);
#2982=EDGE_CURVE('',#2380,#2381,#1477,.T.);
#2983=EDGE_CURVE('',#2197,#2382,#1478,.F.);
#2984=EDGE_CURVE('',#2383,#2382,#1479,.T.);
#2985=EDGE_CURVE('',#2199,#2383,#1480,.T.);
#2986=EDGE_CURVE('',#2382,#2384,#1032,.T.);
#2987=EDGE_CURVE('',#2383,#2384,#1481,.T.);
#2988=EDGE_CURVE('',#2203,#2216,#1033,.T.);
#2989=EDGE_CURVE('',#2385,#2386,#1034,.T.);
#2990=EDGE_CURVE('',#2387,#2385,#1482,.T.);
#2991=EDGE_CURVE('',#2387,#2386,#1483,.T.);
#2992=EDGE_CURVE('',#2385,#2206,#1484,.F.);
#2993=EDGE_CURVE('',#2387,#2205,#1485,.T.);
#2994=EDGE_CURVE('',#2388,#2389,#1035,.T.);
#2995=EDGE_CURVE('',#2390,#2388,#1486,.T.);
#2996=EDGE_CURVE('',#2390,#2389,#1487,.T.);
#2997=EDGE_CURVE('',#2388,#2391,#1488,.F.);
#2998=EDGE_CURVE('',#2392,#2391,#1489,.T.);
#2999=EDGE_CURVE('',#2390,#2392,#1490,.T.);
#3000=EDGE_CURVE('',#2391,#2393,#1036,.T.);
#3001=EDGE_CURVE('',#2392,#2393,#1491,.T.);
#3002=EDGE_CURVE('',#2192,#2196,#1492,.F.);
#3003=EDGE_CURVE('',#2209,#2213,#1493,.F.);
#3004=EDGE_CURVE('',#2186,#2190,#1494,.F.);
#3005=EDGE_CURVE('',#2312,#2381,#1495,.T.);
#3006=EDGE_CURVE('',#2389,#2301,#1496,.T.);
#3007=EDGE_CURVE('',#2386,#2393,#1497,.T.);
#3008=EDGE_CURVE('',#2198,#2207,#1498,.T.);
#3009=EDGE_CURVE('',#2377,#2384,#1499,.T.);
#3010=EDGE_CURVE('',#2394,#2395,#1037,.T.);
#3011=EDGE_CURVE('',#2395,#2396,#1500,.F.);
#3012=EDGE_CURVE('',#2397,#2396,#1038,.T.);
#3013=EDGE_CURVE('',#2397,#2394,#1501,.T.);
#3014=EDGE_CURVE('',#2398,#2399,#1502,.T.);
#3015=EDGE_CURVE('',#2399,#2400,#1039,.T.);
#3016=EDGE_CURVE('',#2401,#2400,#1503,.T.);
#3017=EDGE_CURVE('',#2398,#2401,#1040,.T.);
#3018=EDGE_CURVE('',#2402,#2403,#1504,.T.);
#3019=EDGE_CURVE('',#2403,#2404,#1041,.T.);
#3020=EDGE_CURVE('',#2405,#2404,#1505,.T.);
#3021=EDGE_CURVE('',#2402,#2405,#1042,.T.);
#3022=EDGE_CURVE('',#2406,#2407,#1506,.F.);
#3023=EDGE_CURVE('',#2407,#2408,#1043,.T.);
#3024=EDGE_CURVE('',#2409,#2408,#1507,.F.);
#3025=EDGE_CURVE('',#2406,#2409,#1044,.T.);
#3026=EDGE_CURVE('',#2410,#2411,#1508,.T.);
#3027=EDGE_CURVE('',#2411,#2412,#1045,.T.);
#3028=EDGE_CURVE('',#2413,#2412,#1509,.T.);
#3029=EDGE_CURVE('',#2410,#2413,#1046,.T.);
#3030=EDGE_CURVE('',#2414,#2415,#1047,.T.);
#3031=EDGE_CURVE('',#2415,#2416,#1510,.F.);
#3032=EDGE_CURVE('',#2417,#2416,#1048,.T.);
#3033=EDGE_CURVE('',#2417,#2414,#1511,.T.);
#3034=EDGE_CURVE('',#2418,#2419,#1512,.T.);
#3035=EDGE_CURVE('',#2419,#2420,#1049,.T.);
#3036=EDGE_CURVE('',#2421,#2420,#1513,.T.);
#3037=EDGE_CURVE('',#2418,#2421,#1050,.T.);
#3038=EDGE_CURVE('',#2422,#2423,#1051,.T.);
#3039=EDGE_CURVE('',#2423,#2424,#1514,.F.);
#3040=EDGE_CURVE('',#2425,#2424,#1052,.T.);
#3041=EDGE_CURVE('',#2425,#2422,#1515,.T.);
#3042=EDGE_CURVE('',#2425,#2174,#1516,.T.);
#3043=EDGE_CURVE('',#2422,#2176,#1517,.T.);
#3044=EDGE_CURVE('',#2424,#2426,#1053,.T.);
#3045=EDGE_CURVE('',#2426,#2427,#1518,.T.);
#3046=EDGE_CURVE('',#2427,#2173,#1054,.T.);
#3047=EDGE_CURVE('',#2428,#2429,#1519,.T.);
#3048=EDGE_CURVE('',#2429,#2427,#1520,.T.);
#3049=EDGE_CURVE('',#2426,#2428,#1521,.T.);
#3050=EDGE_CURVE('',#2175,#2429,#1055,.F.);
#3051=EDGE_CURVE('',#2428,#2423,#1056,.F.);
#3052=EDGE_CURVE('',#2430,#2431,#1522,.T.);
#3053=EDGE_CURVE('',#2431,#2432,#1523,.F.);
#3054=EDGE_CURVE('',#2433,#2432,#1524,.T.);
#3055=EDGE_CURVE('',#2433,#2430,#1525,.T.);
#3056=EDGE_CURVE('',#2430,#2418,#1057,.T.);
#3057=EDGE_CURVE('',#2421,#2183,#1526,.T.);
#3058=EDGE_CURVE('',#2182,#2431,#1058,.T.);
#3059=EDGE_CURVE('',#2420,#2184,#1527,.T.);
#3060=EDGE_CURVE('',#2419,#2433,#1059,.F.);
#3061=EDGE_CURVE('',#2432,#2181,#1060,.F.);
#3062=EDGE_CURVE('',#2417,#2154,#1528,.T.);
#3063=EDGE_CURVE('',#2414,#2156,#1529,.T.);
#3064=EDGE_CURVE('',#2416,#2434,#1061,.T.);
#3065=EDGE_CURVE('',#2434,#2435,#1530,.T.);
#3066=EDGE_CURVE('',#2435,#2153,#1062,.T.);
#3067=EDGE_CURVE('',#2436,#2437,#1531,.T.);
#3068=EDGE_CURVE('',#2437,#2435,#1532,.T.);
#3069=EDGE_CURVE('',#2434,#2436,#1533,.T.);
#3070=EDGE_CURVE('',#2155,#2437,#1063,.F.);
#3071=EDGE_CURVE('',#2436,#2415,#1064,.F.);
#3072=EDGE_CURVE('',#2438,#2439,#1534,.T.);
#3073=EDGE_CURVE('',#2439,#2440,#1535,.F.);
#3074=EDGE_CURVE('',#2441,#2440,#1536,.T.);
#3075=EDGE_CURVE('',#2441,#2438,#1537,.T.);
#3076=EDGE_CURVE('',#2438,#2410,#1065,.T.);
#3077=EDGE_CURVE('',#2413,#2167,#1538,.T.);
#3078=EDGE_CURVE('',#2166,#2439,#1066,.T.);
#3079=EDGE_CURVE('',#2412,#2168,#1539,.T.);
#3080=EDGE_CURVE('',#2411,#2441,#1067,.F.);
#3081=EDGE_CURVE('',#2440,#2165,#1068,.F.);
#3082=EDGE_CURVE('',#2442,#2443,#1540,.T.);
#3083=EDGE_CURVE('',#2443,#2444,#1541,.F.);
#3084=EDGE_CURVE('',#2445,#2444,#1542,.T.);
#3085=EDGE_CURVE('',#2445,#2442,#1543,.F.);
#3086=EDGE_CURVE('',#2442,#2406,#1069,.T.);
#3087=EDGE_CURVE('',#2409,#2179,#1544,.T.);
#3088=EDGE_CURVE('',#2178,#2443,#1070,.T.);
#3089=EDGE_CURVE('',#2408,#2180,#1545,.T.);
#3090=EDGE_CURVE('',#2407,#2445,#1071,.F.);
#3091=EDGE_CURVE('',#2444,#2177,#1072,.F.);
#3092=EDGE_CURVE('',#2446,#2447,#1546,.T.);
#3093=EDGE_CURVE('',#2447,#2448,#1547,.F.);
#3094=EDGE_CURVE('',#2449,#2448,#1548,.T.);
#3095=EDGE_CURVE('',#2449,#2446,#1549,.T.);
#3096=EDGE_CURVE('',#2446,#2402,#1073,.T.);
#3097=EDGE_CURVE('',#2405,#2171,#1550,.T.);
#3098=EDGE_CURVE('',#2170,#2447,#1074,.T.);
#3099=EDGE_CURVE('',#2404,#2172,#1551,.T.);
#3100=EDGE_CURVE('',#2403,#2449,#1075,.F.);
#3101=EDGE_CURVE('',#2448,#2169,#1076,.F.);
#3102=EDGE_CURVE('',#2450,#2451,#1552,.T.);
#3103=EDGE_CURVE('',#2451,#2452,#1553,.F.);
#3104=EDGE_CURVE('',#2453,#2452,#1554,.T.);
#3105=EDGE_CURVE('',#2453,#2450,#1555,.T.);
#3106=EDGE_CURVE('',#2450,#2398,#1077,.T.);
#3107=EDGE_CURVE('',#2401,#2163,#1556,.T.);
#3108=EDGE_CURVE('',#2162,#2451,#1078,.T.);
#3109=EDGE_CURVE('',#2400,#2164,#1557,.T.);
#3110=EDGE_CURVE('',#2399,#2453,#1079,.F.);
#3111=EDGE_CURVE('',#2452,#2161,#1080,.F.);
#3112=EDGE_CURVE('',#2397,#2158,#1558,.T.);
#3113=EDGE_CURVE('',#2394,#2160,#1559,.T.);
#3114=EDGE_CURVE('',#2396,#2454,#1081,.T.);
#3115=EDGE_CURVE('',#2454,#2455,#1560,.T.);
#3116=EDGE_CURVE('',#2455,#2157,#1082,.T.);
#3117=EDGE_CURVE('',#2456,#2457,#1561,.T.);
#3118=EDGE_CURVE('',#2457,#2455,#1562,.T.);
#3119=EDGE_CURVE('',#2454,#2456,#1563,.T.);
#3120=EDGE_CURVE('',#2159,#2457,#1083,.F.);
#3121=EDGE_CURVE('',#2456,#2395,#1084,.F.);
#3122=EDGE_CURVE('',#2458,#2459,#1085,.T.);
#3123=EDGE_CURVE('',#2459,#2460,#1564,.T.);
#3124=EDGE_CURVE('',#2460,#2461,#1086,.T.);
#3125=EDGE_CURVE('',#2461,#2462,#1565,.T.);
#3126=EDGE_CURVE('',#2462,#2463,#1087,.T.);
#3127=EDGE_CURVE('',#2463,#2464,#1566,.T.);
#3128=EDGE_CURVE('',#2464,#2465,#1088,.T.);
#3129=EDGE_CURVE('',#2465,#2466,#1567,.T.);
#3130=EDGE_CURVE('',#2466,#2467,#1089,.T.);
#3131=EDGE_CURVE('',#2467,#2468,#1090,.T.);
#3132=EDGE_CURVE('',#2468,#2469,#1568,.T.);
#3133=EDGE_CURVE('',#2469,#2470,#1091,.T.);
#3134=EDGE_CURVE('',#2470,#2471,#1092,.T.);
#3135=EDGE_CURVE('',#2471,#2458,#1569,.T.);
#3136=EDGE_CURVE('',#2472,#2473,#1570,.T.);
#3137=EDGE_CURVE('',#2458,#2473,#1571,.T.);
#3138=EDGE_CURVE('',#2472,#2471,#1572,.F.);
#3139=EDGE_CURVE('',#2474,#2463,#1573,.F.);
#3140=EDGE_CURVE('',#2474,#2475,#1574,.T.);
#3141=EDGE_CURVE('',#2475,#2464,#1575,.T.);
#3142=EDGE_CURVE('',#2476,#2461,#1576,.F.);
#3143=EDGE_CURVE('',#2477,#2476,#1577,.T.);
#3144=EDGE_CURVE('',#2477,#2462,#1578,.T.);
#3145=EDGE_CURVE('',#2478,#2478,#1093,.T.);
#3146=EDGE_CURVE('',#2479,#2479,#1094,.T.);
#3147=EDGE_CURVE('',#2480,#2459,#1579,.F.);
#3148=EDGE_CURVE('',#2481,#2480,#1580,.T.);
#3149=EDGE_CURVE('',#2481,#2460,#1581,.T.);
#3150=EDGE_CURVE('',#2482,#2482,#1095,.T.);
#3151=EDGE_CURVE('',#2482,#2483,#1582,.T.);
#3152=EDGE_CURVE('',#2483,#2483,#1096,.T.);
#3153=EDGE_CURVE('',#2484,#2465,#1583,.F.);
#3154=EDGE_CURVE('',#2484,#2485,#1584,.T.);
#3155=EDGE_CURVE('',#2485,#2466,#1585,.T.);
#3156=EDGE_CURVE('',#2486,#2486,#1097,.T.);
#3157=EDGE_CURVE('',#2486,#2487,#1586,.T.);
#3158=EDGE_CURVE('',#2487,#2487,#1098,.T.);
#3159=EDGE_CURVE('',#2488,#2489,#1587,.T.);
#3160=EDGE_CURVE('',#2490,#2488,#1099,.F.);
#3161=EDGE_CURVE('',#2485,#2490,#1100,.T.);
#3162=EDGE_CURVE('',#2475,#2484,#1101,.F.);
#3163=EDGE_CURVE('',#2477,#2474,#1102,.F.);
#3164=EDGE_CURVE('',#2481,#2476,#1103,.F.);
#3165=EDGE_CURVE('',#2473,#2480,#1104,.F.);
#3166=EDGE_CURVE('',#2491,#2472,#1105,.T.);
#3167=EDGE_CURVE('',#2489,#2491,#1106,.F.);
#3168=EDGE_CURVE('',#2492,#2468,#1588,.T.);
#3169=EDGE_CURVE('',#2492,#2493,#1107,.T.);
#3170=EDGE_CURVE('',#2488,#2493,#1589,.F.);
#3171=EDGE_CURVE('',#2494,#2489,#1590,.T.);
#3172=EDGE_CURVE('',#2494,#2495,#1108,.T.);
#3173=EDGE_CURVE('',#2495,#2496,#1109,.T.);
#3174=EDGE_CURVE('',#2496,#2469,#1591,.T.);
#3175=EDGE_CURVE('',#2479,#2497,#1592,.T.);
#3176=EDGE_CURVE('',#2493,#2497,#150,.T.);
#3177=EDGE_CURVE('',#2497,#2492,#151,.T.);
#3178=EDGE_CURVE('',#2478,#2495,#1593,.T.);
#3179=EDGE_CURVE('',#2496,#2494,#152,.T.);
#3180=EDGE_CURVE('',#2491,#2470,#1594,.T.);
#3181=EDGE_CURVE('',#2490,#2467,#1595,.T.);
#3182=EDGE_CURVE('',#2498,#2499,#1110,.T.);
#3183=EDGE_CURVE('',#2499,#2500,#1596,.T.);
#3184=EDGE_CURVE('',#2500,#2501,#1111,.F.);
#3185=EDGE_CURVE('',#2501,#2500,#1112,.F.);
#3186=EDGE_CURVE('',#2499,#2498,#1113,.T.);
#3187=EDGE_CURVE('',#2502,#2502,#1114,.T.);
#3188=EDGE_CURVE('',#2503,#2503,#1115,.F.);
#3189=EDGE_CURVE('',#2498,#2503,#1116,.T.);
#3190=EDGE_CURVE('',#2502,#2501,#1117,.T.);
#3191=EDGE_CURVE('',#2504,#2504,#1118,.T.);
#3192=EDGE_CURVE('',#2505,#2505,#1119,.T.);
#3193=EDGE_CURVE('',#2506,#2506,#1120,.T.);
#3194=EDGE_CURVE('',#2506,#2504,#1597,.T.);
#3195=EDGE_CURVE('',#2507,#2507,#1121,.T.);
#3196=EDGE_CURVE('',#2505,#2507,#1598,.T.);
#3197=EDGE_CURVE('',#2508,#2509,#1122,.T.);
#3198=EDGE_CURVE('',#2509,#2510,#1599,.T.);
#3199=EDGE_CURVE('',#2510,#2510,#1123,.T.);
#3200=EDGE_CURVE('',#2509,#2508,#1124,.T.);
#3201=EDGE_CURVE('',#2511,#2511,#1125,.T.);
#3202=EDGE_CURVE('',#2508,#2512,#1600,.T.);
#3203=EDGE_CURVE('',#2512,#2512,#1126,.T.);
#3204=EDGE_CURVE('',#2513,#2514,#1127,.T.);
#3205=EDGE_CURVE('',#2514,#2511,#1601,.T.);
#3206=EDGE_CURVE('',#2514,#2513,#1128,.T.);
#3207=EDGE_CURVE('',#2515,#2515,#1129,.T.);
#3208=EDGE_CURVE('',#2515,#2513,#1602,.T.);
#3209=EDGE_CURVE('',#2516,#2517,#1130,.T.);
#3210=EDGE_CURVE('',#2517,#2518,#1603,.T.);
#3211=EDGE_CURVE('',#2518,#2518,#1131,.T.);
#3212=EDGE_CURVE('',#2517,#2516,#1132,.T.);
#3213=EDGE_CURVE('',#2519,#2519,#1133,.T.);
#3214=EDGE_CURVE('',#2520,#2520,#1134,.T.);
#3215=EDGE_CURVE('',#2520,#2516,#1604,.T.);
#3216=EDGE_CURVE('',#2521,#2522,#1135,.T.);
#3217=EDGE_CURVE('',#2522,#2519,#1605,.T.);
#3218=EDGE_CURVE('',#2522,#2521,#1136,.T.);
#3219=EDGE_CURVE('',#2521,#2523,#1606,.T.);
#3220=EDGE_CURVE('',#2523,#2523,#1137,.T.);
#3221=EDGE_CURVE('',#2524,#2524,#1138,.T.);
#3222=EDGE_CURVE('',#2525,#2525,#1139,.T.);
#3223=EDGE_CURVE('',#2525,#2524,#1607,.T.);
#3224=EDGE_CURVE('',#2526,#2526,#1140,.T.);
#3225=EDGE_CURVE('',#2527,#2527,#1141,.T.);
#3226=EDGE_CURVE('',#2527,#2526,#1608,.T.);
#3227=EDGE_CURVE('',#2528,#2528,#1142,.T.);
#3228=EDGE_CURVE('',#2528,#2527,#1609,.T.);
#3229=EDGE_CURVE('',#2529,#2529,#1143,.T.);
#3230=EDGE_CURVE('',#2529,#2528,#1610,.T.);
#3231=EDGE_CURVE('',#2529,#2530,#1611,.T.);
#3232=EDGE_CURVE('',#2530,#2530,#1144,.T.);
#3233=EDGE_CURVE('',#2531,#2531,#1145,.T.);
#3234=EDGE_CURVE('',#2531,#2530,#1612,.T.);
#3235=EDGE_CURVE('',#2532,#2532,#1146,.T.);
#3236=EDGE_CURVE('',#2533,#2533,#1147,.T.);
#3237=EDGE_CURVE('',#2533,#2532,#1613,.T.);
#3238=EDGE_CURVE('',#2534,#2534,#1148,.T.);
#3239=EDGE_CURVE('',#2535,#2535,#1149,.T.);
#3240=EDGE_CURVE('',#2535,#2534,#1614,.T.);
#3241=EDGE_CURVE('',#2536,#2536,#1150,.T.);
#3242=EDGE_CURVE('',#2537,#2537,#1151,.T.);
#3243=EDGE_CURVE('',#2537,#2536,#1615,.T.);
#3244=EDGE_CURVE('',#2538,#2538,#1152,.T.);
#3245=EDGE_CURVE('',#2539,#2539,#1153,.T.);
#3246=EDGE_CURVE('',#2539,#2538,#1616,.T.);
#3247=EDGE_CURVE('',#2540,#2540,#1154,.T.);
#3248=EDGE_CURVE('',#2541,#2541,#1155,.T.);
#3249=EDGE_CURVE('',#2542,#2542,#1156,.T.);
#3250=EDGE_CURVE('',#2542,#2540,#1617,.T.);
#3251=EDGE_CURVE('',#2543,#2543,#1157,.T.);
#3252=EDGE_CURVE('',#2544,#2544,#1158,.T.);
#3253=EDGE_CURVE('',#2544,#2543,#1618,.T.);
#3254=EDGE_CURVE('',#2545,#2545,#1159,.T.);
#3255=EDGE_CURVE('',#2545,#2544,#1619,.T.);
#3256=EDGE_CURVE('',#2546,#2546,#1160,.T.);
#3257=EDGE_CURVE('',#2541,#2546,#1620,.T.);
#3258=EDGE_CURVE('',#2547,#2547,#1161,.T.);
#3259=EDGE_CURVE('',#2548,#2548,#1162,.T.);
#3260=EDGE_CURVE('',#2547,#2549,#1621,.T.);
#3261=EDGE_CURVE('',#2549,#2549,#1163,.T.);
#3262=EDGE_CURVE('',#2550,#2550,#1164,.T.);
#3263=EDGE_CURVE('',#2550,#2548,#1622,.T.);
#3264=EDGE_CURVE('',#2551,#2551,#1165,.T.);
#3265=EDGE_CURVE('',#2552,#2552,#1166,.T.);
#3266=EDGE_CURVE('',#2551,#2553,#1623,.T.);
#3267=EDGE_CURVE('',#2553,#2553,#1167,.T.);
#3268=EDGE_CURVE('',#2554,#2554,#1168,.T.);
#3269=EDGE_CURVE('',#2555,#2555,#1169,.T.);
#3270=EDGE_CURVE('',#2555,#2554,#1624,.T.);
#3271=EDGE_CURVE('',#2555,#2556,#1625,.T.);
#3272=EDGE_CURVE('',#2556,#2556,#1170,.T.);
#3273=EDGE_CURVE('',#2557,#2557,#1171,.T.);
#3274=EDGE_CURVE('',#2552,#2557,#1626,.T.);
#3275=ORIENTED_EDGE('',*,*,#2558,.T.);
#3276=ORIENTED_EDGE('',*,*,#2559,.T.);
#3277=ORIENTED_EDGE('',*,*,#2560,.T.);
#3278=ORIENTED_EDGE('',*,*,#2561,.T.);
#3279=ORIENTED_EDGE('',*,*,#2562,.T.);
#3280=ORIENTED_EDGE('',*,*,#2563,.T.);
#3281=ORIENTED_EDGE('',*,*,#2564,.T.);
#3282=ORIENTED_EDGE('',*,*,#2565,.T.);
#3283=ORIENTED_EDGE('',*,*,#2566,.T.);
#3284=ORIENTED_EDGE('',*,*,#2567,.T.);
#3285=ORIENTED_EDGE('',*,*,#2568,.T.);
#3286=ORIENTED_EDGE('',*,*,#2569,.T.);
#3287=ORIENTED_EDGE('',*,*,#2570,.T.);
#3288=ORIENTED_EDGE('',*,*,#2571,.T.);
#3289=ORIENTED_EDGE('',*,*,#2572,.F.);
#3290=ORIENTED_EDGE('',*,*,#2573,.T.);
#3291=ORIENTED_EDGE('',*,*,#2566,.F.);
#3292=ORIENTED_EDGE('',*,*,#2574,.T.);
#3293=ORIENTED_EDGE('',*,*,#2575,.T.);
#3294=ORIENTED_EDGE('',*,*,#2576,.F.);
#3295=ORIENTED_EDGE('',*,*,#2577,.T.);
#3296=ORIENTED_EDGE('',*,*,#2560,.F.);
#3297=ORIENTED_EDGE('',*,*,#2578,.T.);
#3298=ORIENTED_EDGE('',*,*,#2579,.T.);
#3299=ORIENTED_EDGE('',*,*,#2580,.T.);
#3300=ORIENTED_EDGE('',*,*,#2562,.F.);
#3301=ORIENTED_EDGE('',*,*,#2581,.T.);
#3302=ORIENTED_EDGE('',*,*,#2582,.T.);
#3303=ORIENTED_EDGE('',*,*,#2583,.T.);
#3304=ORIENTED_EDGE('',*,*,#2584,.T.);
#3305=ORIENTED_EDGE('',*,*,#2585,.T.);
#3306=ORIENTED_EDGE('',*,*,#2564,.F.);
#3307=ORIENTED_EDGE('',*,*,#2586,.T.);
#3308=ORIENTED_EDGE('',*,*,#2587,.T.);
#3309=ORIENTED_EDGE('',*,*,#2588,.F.);
#3310=ORIENTED_EDGE('',*,*,#2587,.F.);
#3311=ORIENTED_EDGE('',*,*,#2589,.T.);
#3312=ORIENTED_EDGE('',*,*,#2590,.F.);
#3313=ORIENTED_EDGE('',*,*,#2591,.T.);
#3314=ORIENTED_EDGE('',*,*,#2558,.F.);
#3315=ORIENTED_EDGE('',*,*,#2592,.T.);
#3316=ORIENTED_EDGE('',*,*,#2593,.T.);
#3317=ORIENTED_EDGE('',*,*,#2594,.F.);
#3318=ORIENTED_EDGE('',*,*,#2593,.F.);
#3319=ORIENTED_EDGE('',*,*,#2595,.T.);
#3320=ORIENTED_EDGE('',*,*,#2596,.T.);
#3321=ORIENTED_EDGE('',*,*,#2597,.T.);
#3322=ORIENTED_EDGE('',*,*,#2572,.T.);
#3323=ORIENTED_EDGE('',*,*,#2598,.T.);
#3324=ORIENTED_EDGE('',*,*,#2584,.F.);
#3325=ORIENTED_EDGE('',*,*,#2599,.T.);
#3326=ORIENTED_EDGE('',*,*,#2579,.F.);
#3327=ORIENTED_EDGE('',*,*,#2600,.T.);
#3328=ORIENTED_EDGE('',*,*,#2576,.T.);
#3329=ORIENTED_EDGE('',*,*,#2601,.T.);
#3330=ORIENTED_EDGE('',*,*,#2590,.T.);
#3331=ORIENTED_EDGE('',*,*,#2602,.T.);
#3332=ORIENTED_EDGE('',*,*,#2603,.T.);
#3333=ORIENTED_EDGE('',*,*,#2588,.T.);
#3334=ORIENTED_EDGE('',*,*,#2594,.T.);
#3335=ORIENTED_EDGE('',*,*,#2592,.F.);
#3336=ORIENTED_EDGE('',*,*,#2586,.F.);
#3337=ORIENTED_EDGE('',*,*,#2591,.F.);
#3338=ORIENTED_EDGE('',*,*,#2601,.F.);
#3339=ORIENTED_EDGE('',*,*,#2575,.F.);
#3340=ORIENTED_EDGE('',*,*,#2559,.F.);
#3341=ORIENTED_EDGE('',*,*,#2577,.F.);
#3342=ORIENTED_EDGE('',*,*,#2600,.F.);
#3343=ORIENTED_EDGE('',*,*,#2578,.F.);
#3344=ORIENTED_EDGE('',*,*,#2561,.F.);
#3345=ORIENTED_EDGE('',*,*,#2580,.F.);
#3346=ORIENTED_EDGE('',*,*,#2599,.F.);
#3347=ORIENTED_EDGE('',*,*,#2583,.F.);
#3348=ORIENTED_EDGE('',*,*,#2563,.F.);
#3349=ORIENTED_EDGE('',*,*,#2585,.F.);
#3350=ORIENTED_EDGE('',*,*,#2598,.F.);
#3351=ORIENTED_EDGE('',*,*,#2574,.F.);
#3352=ORIENTED_EDGE('',*,*,#2565,.F.);
#3353=ORIENTED_EDGE('',*,*,#2604,.F.);
#3354=ORIENTED_EDGE('',*,*,#2605,.F.);
#3355=ORIENTED_EDGE('',*,*,#2606,.F.);
#3356=ORIENTED_EDGE('',*,*,#2607,.T.);
#3357=ORIENTED_EDGE('',*,*,#2595,.F.);
#3358=ORIENTED_EDGE('',*,*,#2608,.T.);
#3359=ORIENTED_EDGE('',*,*,#2609,.F.);
#3360=ORIENTED_EDGE('',*,*,#2610,.T.);
#3361=ORIENTED_EDGE('',*,*,#2569,.F.);
#3362=ORIENTED_EDGE('',*,*,#2582,.F.);
#3363=ORIENTED_EDGE('',*,*,#2611,.T.);
#3364=ORIENTED_EDGE('',*,*,#2612,.T.);
#3365=ORIENTED_EDGE('',*,*,#2609,.T.);
#3366=ORIENTED_EDGE('',*,*,#2613,.T.);
#3367=ORIENTED_EDGE('',*,*,#2611,.F.);
#3368=ORIENTED_EDGE('',*,*,#2581,.F.);
#3369=ORIENTED_EDGE('',*,*,#2614,.T.);
#3370=ORIENTED_EDGE('',*,*,#2605,.T.);
#3371=ORIENTED_EDGE('',*,*,#2615,.T.);
#3372=ORIENTED_EDGE('',*,*,#2606,.T.);
#3373=ORIENTED_EDGE('',*,*,#2614,.F.);
#3374=ORIENTED_EDGE('',*,*,#2604,.T.);
#3375=ORIENTED_EDGE('',*,*,#2568,.F.);
#3376=ORIENTED_EDGE('',*,*,#2616,.F.);
#3377=ORIENTED_EDGE('',*,*,#2596,.F.);
#3378=ORIENTED_EDGE('',*,*,#2607,.F.);
#3379=ORIENTED_EDGE('',*,*,#2615,.F.);
#3380=ORIENTED_EDGE('',*,*,#2573,.F.);
#3381=ORIENTED_EDGE('',*,*,#2597,.F.);
#3382=ORIENTED_EDGE('',*,*,#2616,.T.);
#3383=ORIENTED_EDGE('',*,*,#2567,.F.);
#3384=ORIENTED_EDGE('',*,*,#2617,.T.);
#3385=ORIENTED_EDGE('',*,*,#2570,.F.);
#3386=ORIENTED_EDGE('',*,*,#2610,.F.);
#3387=ORIENTED_EDGE('',*,*,#2612,.F.);
#3388=ORIENTED_EDGE('',*,*,#2613,.F.);
#3389=ORIENTED_EDGE('',*,*,#2608,.F.);
#3390=ORIENTED_EDGE('',*,*,#2603,.F.);
#3391=ORIENTED_EDGE('',*,*,#2617,.F.);
#3392=ORIENTED_EDGE('',*,*,#2602,.F.);
#3393=ORIENTED_EDGE('',*,*,#2589,.F.);
#3394=ORIENTED_EDGE('',*,*,#2571,.F.);
#3395=ORIENTED_EDGE('',*,*,#2618,.F.);
#3396=ORIENTED_EDGE('',*,*,#2619,.F.);
#3397=ORIENTED_EDGE('',*,*,#2620,.F.);
#3398=ORIENTED_EDGE('',*,*,#2621,.F.);
#3399=ORIENTED_EDGE('',*,*,#2622,.F.);
#3400=ORIENTED_EDGE('',*,*,#2623,.F.);
#3401=ORIENTED_EDGE('',*,*,#2624,.F.);
#3402=ORIENTED_EDGE('',*,*,#2625,.T.);
#3403=ORIENTED_EDGE('',*,*,#2626,.F.);
#3404=ORIENTED_EDGE('',*,*,#2625,.F.);
#3405=ORIENTED_EDGE('',*,*,#2627,.F.);
#3406=ORIENTED_EDGE('',*,*,#2619,.T.);
#3407=ORIENTED_EDGE('',*,*,#2621,.T.);
#3408=ORIENTED_EDGE('',*,*,#2628,.T.);
#3409=ORIENTED_EDGE('',*,*,#2629,.F.);
#3410=ORIENTED_EDGE('',*,*,#2630,.F.);
#3411=ORIENTED_EDGE('',*,*,#2631,.F.);
#3412=ORIENTED_EDGE('',*,*,#2632,.T.);
#3413=ORIENTED_EDGE('',*,*,#2633,.T.);
#3414=ORIENTED_EDGE('',*,*,#2634,.F.);
#3415=ORIENTED_EDGE('',*,*,#2623,.T.);
#3416=ORIENTED_EDGE('',*,*,#2635,.F.);
#3417=ORIENTED_EDGE('',*,*,#2636,.F.);
#3418=ORIENTED_EDGE('',*,*,#2637,.T.);
#3419=ORIENTED_EDGE('',*,*,#2638,.T.);
#3420=ORIENTED_EDGE('',*,*,#2639,.F.);
#3421=ORIENTED_EDGE('',*,*,#2640,.T.);
#3422=ORIENTED_EDGE('',*,*,#2641,.T.);
#3423=ORIENTED_EDGE('',*,*,#2622,.T.);
#3424=ORIENTED_EDGE('',*,*,#2626,.T.);
#3425=ORIENTED_EDGE('',*,*,#2618,.T.);
#3426=ORIENTED_EDGE('',*,*,#2634,.T.);
#3427=ORIENTED_EDGE('',*,*,#2642,.F.);
#3428=ORIENTED_EDGE('',*,*,#2643,.F.);
#3429=ORIENTED_EDGE('',*,*,#2644,.T.);
#3430=ORIENTED_EDGE('',*,*,#2635,.T.);
#3431=ORIENTED_EDGE('',*,*,#2645,.T.);
#3432=ORIENTED_EDGE('',*,*,#2646,.F.);
#3433=ORIENTED_EDGE('',*,*,#2647,.F.);
#3434=ORIENTED_EDGE('',*,*,#2648,.F.);
#3435=ORIENTED_EDGE('',*,*,#2646,.T.);
#3436=ORIENTED_EDGE('',*,*,#2649,.F.);
#3437=ORIENTED_EDGE('',*,*,#2650,.F.);
#3438=ORIENTED_EDGE('',*,*,#2651,.T.);
#3439=ORIENTED_EDGE('',*,*,#2652,.T.);
#3440=ORIENTED_EDGE('',*,*,#2653,.T.);
#3441=ORIENTED_EDGE('',*,*,#2650,.T.);
#3442=ORIENTED_EDGE('',*,*,#2654,.T.);
#3443=ORIENTED_EDGE('',*,*,#2655,.F.);
#3444=ORIENTED_EDGE('',*,*,#2636,.T.);
#3445=ORIENTED_EDGE('',*,*,#2644,.F.);
#3446=ORIENTED_EDGE('',*,*,#2656,.F.);
#3447=ORIENTED_EDGE('',*,*,#2657,.F.);
#3448=ORIENTED_EDGE('',*,*,#2658,.T.);
#3449=ORIENTED_EDGE('',*,*,#2659,.T.);
#3450=ORIENTED_EDGE('',*,*,#2660,.T.);
#3451=ORIENTED_EDGE('',*,*,#2661,.F.);
#3452=ORIENTED_EDGE('',*,*,#2662,.T.);
#3453=ORIENTED_EDGE('',*,*,#2663,.T.);
#3454=ORIENTED_EDGE('',*,*,#2664,.T.);
#3455=ORIENTED_EDGE('',*,*,#2665,.T.);
#3456=ORIENTED_EDGE('',*,*,#2666,.F.);
#3457=ORIENTED_EDGE('',*,*,#2667,.F.);
#3458=ORIENTED_EDGE('',*,*,#2668,.T.);
#3459=ORIENTED_EDGE('',*,*,#2669,.T.);
#3460=ORIENTED_EDGE('',*,*,#2670,.F.);
#3461=ORIENTED_EDGE('',*,*,#2671,.F.);
#3462=ORIENTED_EDGE('',*,*,#2672,.T.);
#3463=ORIENTED_EDGE('',*,*,#2673,.T.);
#3464=ORIENTED_EDGE('',*,*,#2674,.F.);
#3465=ORIENTED_EDGE('',*,*,#2675,.F.);
#3466=ORIENTED_EDGE('',*,*,#2676,.T.);
#3467=ORIENTED_EDGE('',*,*,#2677,.F.);
#3468=ORIENTED_EDGE('',*,*,#2678,.T.);
#3469=ORIENTED_EDGE('',*,*,#2679,.T.);
#3470=ORIENTED_EDGE('',*,*,#2680,.T.);
#3471=ORIENTED_EDGE('',*,*,#2681,.T.);
#3472=ORIENTED_EDGE('',*,*,#2682,.F.);
#3473=ORIENTED_EDGE('',*,*,#2683,.F.);
#3474=ORIENTED_EDGE('',*,*,#2684,.T.);
#3475=ORIENTED_EDGE('',*,*,#2685,.T.);
#3476=ORIENTED_EDGE('',*,*,#2686,.F.);
#3477=ORIENTED_EDGE('',*,*,#2687,.F.);
#3478=ORIENTED_EDGE('',*,*,#2688,.T.);
#3479=ORIENTED_EDGE('',*,*,#2689,.F.);
#3480=ORIENTED_EDGE('',*,*,#2690,.T.);
#3481=ORIENTED_EDGE('',*,*,#2691,.T.);
#3482=ORIENTED_EDGE('',*,*,#2692,.F.);
#3483=ORIENTED_EDGE('',*,*,#2693,.T.);
#3484=ORIENTED_EDGE('',*,*,#2694,.F.);
#3485=ORIENTED_EDGE('',*,*,#2695,.F.);
#3486=ORIENTED_EDGE('',*,*,#2696,.T.);
#3487=ORIENTED_EDGE('',*,*,#2697,.T.);
#3488=ORIENTED_EDGE('',*,*,#2698,.F.);
#3489=ORIENTED_EDGE('',*,*,#2699,.T.);
#3490=ORIENTED_EDGE('',*,*,#2700,.F.);
#3491=ORIENTED_EDGE('',*,*,#2701,.F.);
#3492=ORIENTED_EDGE('',*,*,#2702,.F.);
#3493=ORIENTED_EDGE('',*,*,#2703,.T.);
#3494=ORIENTED_EDGE('',*,*,#2704,.F.);
#3495=ORIENTED_EDGE('',*,*,#2705,.F.);
#3496=ORIENTED_EDGE('',*,*,#2706,.T.);
#3497=ORIENTED_EDGE('',*,*,#2705,.T.);
#3498=ORIENTED_EDGE('',*,*,#2707,.T.);
#3499=ORIENTED_EDGE('',*,*,#2708,.F.);
#3500=ORIENTED_EDGE('',*,*,#2709,.F.);
#3501=ORIENTED_EDGE('',*,*,#2710,.T.);
#3502=ORIENTED_EDGE('',*,*,#2711,.T.);
#3503=ORIENTED_EDGE('',*,*,#2712,.F.);
#3504=ORIENTED_EDGE('',*,*,#2713,.F.);
#3505=ORIENTED_EDGE('',*,*,#2714,.T.);
#3506=ORIENTED_EDGE('',*,*,#2715,.T.);
#3507=ORIENTED_EDGE('',*,*,#2716,.F.);
#3508=ORIENTED_EDGE('',*,*,#2717,.T.);
#3509=ORIENTED_EDGE('',*,*,#2718,.F.);
#3510=ORIENTED_EDGE('',*,*,#2719,.F.);
#3511=ORIENTED_EDGE('',*,*,#2720,.T.);
#3512=ORIENTED_EDGE('',*,*,#2692,.T.);
#3513=ORIENTED_EDGE('',*,*,#2721,.F.);
#3514=ORIENTED_EDGE('',*,*,#2690,.F.);
#3515=ORIENTED_EDGE('',*,*,#2722,.T.);
#3516=ORIENTED_EDGE('',*,*,#2698,.T.);
#3517=ORIENTED_EDGE('',*,*,#2723,.F.);
#3518=ORIENTED_EDGE('',*,*,#2696,.F.);
#3519=ORIENTED_EDGE('',*,*,#2724,.T.);
#3520=ORIENTED_EDGE('',*,*,#2706,.F.);
#3521=ORIENTED_EDGE('',*,*,#2709,.T.);
#3522=ORIENTED_EDGE('',*,*,#2725,.T.);
#3523=ORIENTED_EDGE('',*,*,#2726,.T.);
#3524=ORIENTED_EDGE('',*,*,#2716,.T.);
#3525=ORIENTED_EDGE('',*,*,#2727,.F.);
#3526=ORIENTED_EDGE('',*,*,#2714,.F.);
#3527=ORIENTED_EDGE('',*,*,#2728,.F.);
#3528=ORIENTED_EDGE('',*,*,#2729,.T.);
#3529=ORIENTED_EDGE('',*,*,#2730,.T.);
#3530=ORIENTED_EDGE('',*,*,#2731,.T.);
#3531=ORIENTED_EDGE('',*,*,#2648,.T.);
#3532=ORIENTED_EDGE('',*,*,#2732,.F.);
#3533=ORIENTED_EDGE('',*,*,#2640,.F.);
#3534=ORIENTED_EDGE('',*,*,#2633,.F.);
#3535=ORIENTED_EDGE('',*,*,#2733,.T.);
#3536=ORIENTED_EDGE('',*,*,#2734,.T.);
#3537=ORIENTED_EDGE('',*,*,#2642,.T.);
#3538=ORIENTED_EDGE('',*,*,#2735,.F.);
#3539=ORIENTED_EDGE('',*,*,#2736,.T.);
#3540=ORIENTED_EDGE('',*,*,#2737,.T.);
#3541=ORIENTED_EDGE('',*,*,#2738,.T.);
#3542=ORIENTED_EDGE('',*,*,#2739,.T.);
#3543=ORIENTED_EDGE('',*,*,#2740,.F.);
#3544=ORIENTED_EDGE('',*,*,#2741,.F.);
#3545=ORIENTED_EDGE('',*,*,#2742,.T.);
#3546=ORIENTED_EDGE('',*,*,#2743,.F.);
#3547=ORIENTED_EDGE('',*,*,#2744,.T.);
#3548=ORIENTED_EDGE('',*,*,#2745,.T.);
#3549=ORIENTED_EDGE('',*,*,#2746,.T.);
#3550=ORIENTED_EDGE('',*,*,#2747,.T.);
#3551=ORIENTED_EDGE('',*,*,#2748,.F.);
#3552=ORIENTED_EDGE('',*,*,#2749,.F.);
#3553=ORIENTED_EDGE('',*,*,#2750,.T.);
#3554=ORIENTED_EDGE('',*,*,#2751,.T.);
#3555=ORIENTED_EDGE('',*,*,#2752,.F.);
#3556=ORIENTED_EDGE('',*,*,#2753,.F.);
#3557=ORIENTED_EDGE('',*,*,#2754,.T.);
#3558=ORIENTED_EDGE('',*,*,#2755,.F.);
#3559=ORIENTED_EDGE('',*,*,#2756,.T.);
#3560=ORIENTED_EDGE('',*,*,#2757,.T.);
#3561=ORIENTED_EDGE('',*,*,#2758,.T.);
#3562=ORIENTED_EDGE('',*,*,#2759,.F.);
#3563=ORIENTED_EDGE('',*,*,#2760,.T.);
#3564=ORIENTED_EDGE('',*,*,#2761,.T.);
#3565=ORIENTED_EDGE('',*,*,#2762,.T.);
#3566=ORIENTED_EDGE('',*,*,#2763,.F.);
#3567=ORIENTED_EDGE('',*,*,#2764,.T.);
#3568=ORIENTED_EDGE('',*,*,#2765,.T.);
#3569=ORIENTED_EDGE('',*,*,#2766,.T.);
#3570=ORIENTED_EDGE('',*,*,#2767,.F.);
#3571=ORIENTED_EDGE('',*,*,#2768,.T.);
#3572=ORIENTED_EDGE('',*,*,#2769,.T.);
#3573=ORIENTED_EDGE('',*,*,#2770,.F.);
#3574=ORIENTED_EDGE('',*,*,#2771,.T.);
#3575=ORIENTED_EDGE('',*,*,#2772,.F.);
#3576=ORIENTED_EDGE('',*,*,#2773,.F.);
#3577=ORIENTED_EDGE('',*,*,#2774,.T.);
#3578=ORIENTED_EDGE('',*,*,#2775,.F.);
#3579=ORIENTED_EDGE('',*,*,#2776,.T.);
#3580=ORIENTED_EDGE('',*,*,#2777,.T.);
#3581=ORIENTED_EDGE('',*,*,#2778,.F.);
#3582=ORIENTED_EDGE('',*,*,#2779,.F.);
#3583=ORIENTED_EDGE('',*,*,#2780,.T.);
#3584=ORIENTED_EDGE('',*,*,#2781,.T.);
#3585=ORIENTED_EDGE('',*,*,#2782,.F.);
#3586=ORIENTED_EDGE('',*,*,#2783,.F.);
#3587=ORIENTED_EDGE('',*,*,#2784,.T.);
#3588=ORIENTED_EDGE('',*,*,#2785,.T.);
#3589=ORIENTED_EDGE('',*,*,#2786,.F.);
#3590=ORIENTED_EDGE('',*,*,#2787,.F.);
#3591=ORIENTED_EDGE('',*,*,#2788,.F.);
#3592=ORIENTED_EDGE('',*,*,#2789,.T.);
#3593=ORIENTED_EDGE('',*,*,#2790,.T.);
#3594=ORIENTED_EDGE('',*,*,#2791,.F.);
#3595=ORIENTED_EDGE('',*,*,#2792,.T.);
#3596=ORIENTED_EDGE('',*,*,#2793,.F.);
#3597=ORIENTED_EDGE('',*,*,#2794,.T.);
#3598=ORIENTED_EDGE('',*,*,#2795,.T.);
#3599=ORIENTED_EDGE('',*,*,#2796,.F.);
#3600=ORIENTED_EDGE('',*,*,#2797,.F.);
#3601=ORIENTED_EDGE('',*,*,#2798,.F.);
#3602=ORIENTED_EDGE('',*,*,#2769,.F.);
#3603=ORIENTED_EDGE('',*,*,#2799,.T.);
#3604=ORIENTED_EDGE('',*,*,#2772,.T.);
#3605=ORIENTED_EDGE('',*,*,#2800,.F.);
#3606=ORIENTED_EDGE('',*,*,#2801,.F.);
#3607=ORIENTED_EDGE('',*,*,#2802,.T.);
#3608=ORIENTED_EDGE('',*,*,#2775,.T.);
#3609=ORIENTED_EDGE('',*,*,#2803,.F.);
#3610=ORIENTED_EDGE('',*,*,#2790,.F.);
#3611=ORIENTED_EDGE('',*,*,#2804,.T.);
#3612=ORIENTED_EDGE('',*,*,#2793,.T.);
#3613=ORIENTED_EDGE('',*,*,#2805,.F.);
#3614=ORIENTED_EDGE('',*,*,#2806,.T.);
#3615=ORIENTED_EDGE('',*,*,#2807,.F.);
#3616=ORIENTED_EDGE('',*,*,#2797,.T.);
#3617=ORIENTED_EDGE('',*,*,#2808,.T.);
#3618=ORIENTED_EDGE('',*,*,#2809,.T.);
#3619=ORIENTED_EDGE('',*,*,#2810,.F.);
#3620=ORIENTED_EDGE('',*,*,#2787,.T.);
#3621=ORIENTED_EDGE('',*,*,#2811,.T.);
#3622=ORIENTED_EDGE('',*,*,#2812,.T.);
#3623=ORIENTED_EDGE('',*,*,#2813,.F.);
#3624=ORIENTED_EDGE('',*,*,#2783,.T.);
#3625=ORIENTED_EDGE('',*,*,#2814,.T.);
#3626=ORIENTED_EDGE('',*,*,#2815,.T.);
#3627=ORIENTED_EDGE('',*,*,#2816,.F.);
#3628=ORIENTED_EDGE('',*,*,#2779,.T.);
#3629=ORIENTED_EDGE('',*,*,#2817,.T.);
#3630=ORIENTED_EDGE('',*,*,#2818,.F.);
#3631=ORIENTED_EDGE('',*,*,#2819,.T.);
#3632=ORIENTED_EDGE('',*,*,#2820,.F.);
#3633=ORIENTED_EDGE('',*,*,#2821,.T.);
#3634=ORIENTED_EDGE('',*,*,#2822,.T.);
#3635=ORIENTED_EDGE('',*,*,#2823,.F.);
#3636=ORIENTED_EDGE('',*,*,#2629,.T.);
#3637=ORIENTED_EDGE('',*,*,#2824,.F.);
#3638=ORIENTED_EDGE('',*,*,#2825,.T.);
#3639=ORIENTED_EDGE('',*,*,#2637,.F.);
#3640=ORIENTED_EDGE('',*,*,#2655,.T.);
#3641=ORIENTED_EDGE('',*,*,#2826,.T.);
#3642=ORIENTED_EDGE('',*,*,#2733,.F.);
#3643=ORIENTED_EDGE('',*,*,#2632,.F.);
#3644=ORIENTED_EDGE('',*,*,#2827,.F.);
#3645=ORIENTED_EDGE('',*,*,#2729,.F.);
#3646=ORIENTED_EDGE('',*,*,#2828,.F.);
#3647=ORIENTED_EDGE('',*,*,#2829,.F.);
#3648=ORIENTED_EDGE('',*,*,#2654,.F.);
#3649=ORIENTED_EDGE('',*,*,#2649,.T.);
#3650=ORIENTED_EDGE('',*,*,#2645,.F.);
#3651=ORIENTED_EDGE('',*,*,#2731,.F.);
#3652=ORIENTED_EDGE('',*,*,#2639,.T.);
#3653=ORIENTED_EDGE('',*,*,#2830,.T.);
#3654=ORIENTED_EDGE('',*,*,#2831,.F.);
#3655=ORIENTED_EDGE('',*,*,#2832,.F.);
#3656=ORIENTED_EDGE('',*,*,#2630,.T.);
#3657=ORIENTED_EDGE('',*,*,#2823,.T.);
#3658=ORIENTED_EDGE('',*,*,#2833,.T.);
#3659=ORIENTED_EDGE('',*,*,#2834,.F.);
#3660=ORIENTED_EDGE('',*,*,#2835,.T.);
#3661=ORIENTED_EDGE('',*,*,#2836,.T.);
#3662=ORIENTED_EDGE('',*,*,#2805,.T.);
#3663=ORIENTED_EDGE('',*,*,#2837,.F.);
#3664=ORIENTED_EDGE('',*,*,#2837,.T.);
#3665=ORIENTED_EDGE('',*,*,#2820,.T.);
#3666=ORIENTED_EDGE('',*,*,#2838,.F.);
#3667=ORIENTED_EDGE('',*,*,#2730,.F.);
#3668=ORIENTED_EDGE('',*,*,#2839,.F.);
#3669=ORIENTED_EDGE('',*,*,#2840,.F.);
#3670=ORIENTED_EDGE('',*,*,#2841,.F.);
#3671=ORIENTED_EDGE('',*,*,#2842,.F.);
#3672=ORIENTED_EDGE('',*,*,#2843,.F.);
#3673=ORIENTED_EDGE('',*,*,#2624,.T.);
#3674=ORIENTED_EDGE('',*,*,#2641,.F.);
#3675=ORIENTED_EDGE('',*,*,#2732,.T.);
#3676=ORIENTED_EDGE('',*,*,#2647,.T.);
#3677=ORIENTED_EDGE('',*,*,#2651,.F.);
#3678=ORIENTED_EDGE('',*,*,#2653,.F.);
#3679=ORIENTED_EDGE('',*,*,#2844,.T.);
#3680=ORIENTED_EDGE('',*,*,#2845,.F.);
#3681=ORIENTED_EDGE('',*,*,#2719,.T.);
#3682=ORIENTED_EDGE('',*,*,#2838,.T.);
#3683=ORIENTED_EDGE('',*,*,#2819,.F.);
#3684=ORIENTED_EDGE('',*,*,#2846,.F.);
#3685=ORIENTED_EDGE('',*,*,#2847,.F.);
#3686=ORIENTED_EDGE('',*,*,#2848,.T.);
#3687=ORIENTED_EDGE('',*,*,#2849,.T.);
#3688=ORIENTED_EDGE('',*,*,#2821,.F.);
#3689=ORIENTED_EDGE('',*,*,#2628,.F.);
#3690=ORIENTED_EDGE('',*,*,#2620,.T.);
#3691=ORIENTED_EDGE('',*,*,#2627,.T.);
#3692=ORIENTED_EDGE('',*,*,#2734,.F.);
#3693=ORIENTED_EDGE('',*,*,#2826,.F.);
#3694=ORIENTED_EDGE('',*,*,#2656,.T.);
#3695=ORIENTED_EDGE('',*,*,#2643,.T.);
#3696=ORIENTED_EDGE('',*,*,#2850,.F.);
#3697=ORIENTED_EDGE('',*,*,#2851,.F.);
#3698=ORIENTED_EDGE('',*,*,#2852,.F.);
#3699=ORIENTED_EDGE('',*,*,#2853,.F.);
#3700=ORIENTED_EDGE('',*,*,#2854,.F.);
#3701=ORIENTED_EDGE('',*,*,#2855,.T.);
#3702=ORIENTED_EDGE('',*,*,#2830,.F.);
#3703=ORIENTED_EDGE('',*,*,#2638,.F.);
#3704=ORIENTED_EDGE('',*,*,#2825,.F.);
#3705=ORIENTED_EDGE('',*,*,#2827,.T.);
#3706=ORIENTED_EDGE('',*,*,#2631,.T.);
#3707=ORIENTED_EDGE('',*,*,#2832,.T.);
#3708=ORIENTED_EDGE('',*,*,#2856,.F.);
#3709=ORIENTED_EDGE('',*,*,#2824,.T.);
#3710=ORIENTED_EDGE('',*,*,#2856,.T.);
#3711=ORIENTED_EDGE('',*,*,#2831,.T.);
#3712=ORIENTED_EDGE('',*,*,#2855,.F.);
#3713=ORIENTED_EDGE('',*,*,#2854,.T.);
#3714=ORIENTED_EDGE('',*,*,#2857,.T.);
#3715=ORIENTED_EDGE('',*,*,#2843,.T.);
#3716=ORIENTED_EDGE('',*,*,#2857,.F.);
#3717=ORIENTED_EDGE('',*,*,#2853,.T.);
#3718=ORIENTED_EDGE('',*,*,#2858,.T.);
#3719=ORIENTED_EDGE('',*,*,#2842,.T.);
#3720=ORIENTED_EDGE('',*,*,#2858,.F.);
#3721=ORIENTED_EDGE('',*,*,#2852,.T.);
#3722=ORIENTED_EDGE('',*,*,#2859,.T.);
#3723=ORIENTED_EDGE('',*,*,#2841,.T.);
#3724=ORIENTED_EDGE('',*,*,#2859,.F.);
#3725=ORIENTED_EDGE('',*,*,#2851,.T.);
#3726=ORIENTED_EDGE('',*,*,#2860,.T.);
#3727=ORIENTED_EDGE('',*,*,#2840,.T.);
#3728=ORIENTED_EDGE('',*,*,#2860,.F.);
#3729=ORIENTED_EDGE('',*,*,#2850,.T.);
#3730=ORIENTED_EDGE('',*,*,#2861,.T.);
#3731=ORIENTED_EDGE('',*,*,#2839,.T.);
#3732=ORIENTED_EDGE('',*,*,#2861,.F.);
#3733=ORIENTED_EDGE('',*,*,#2834,.T.);
#3734=ORIENTED_EDGE('',*,*,#2862,.T.);
#3735=ORIENTED_EDGE('',*,*,#2848,.F.);
#3736=ORIENTED_EDGE('',*,*,#2863,.F.);
#3737=ORIENTED_EDGE('',*,*,#2864,.F.);
#3738=ORIENTED_EDGE('',*,*,#2865,.T.);
#3739=ORIENTED_EDGE('',*,*,#2801,.T.);
#3740=ORIENTED_EDGE('',*,*,#2866,.F.);
#3741=ORIENTED_EDGE('',*,*,#2776,.F.);
#3742=ORIENTED_EDGE('',*,*,#2816,.T.);
#3743=ORIENTED_EDGE('',*,*,#2778,.T.);
#3744=ORIENTED_EDGE('',*,*,#2867,.T.);
#3745=ORIENTED_EDGE('',*,*,#2817,.F.);
#3746=ORIENTED_EDGE('',*,*,#2868,.F.);
#3747=ORIENTED_EDGE('',*,*,#2780,.F.);
#3748=ORIENTED_EDGE('',*,*,#2813,.T.);
#3749=ORIENTED_EDGE('',*,*,#2782,.T.);
#3750=ORIENTED_EDGE('',*,*,#2869,.T.);
#3751=ORIENTED_EDGE('',*,*,#2814,.F.);
#3752=ORIENTED_EDGE('',*,*,#2870,.F.);
#3753=ORIENTED_EDGE('',*,*,#2871,.F.);
#3754=ORIENTED_EDGE('',*,*,#2872,.T.);
#3755=ORIENTED_EDGE('',*,*,#2871,.T.);
#3756=ORIENTED_EDGE('',*,*,#2873,.T.);
#3757=ORIENTED_EDGE('',*,*,#2874,.F.);
#3758=ORIENTED_EDGE('',*,*,#2875,.F.);
#3759=ORIENTED_EDGE('',*,*,#2874,.T.);
#3760=ORIENTED_EDGE('',*,*,#2876,.T.);
#3761=ORIENTED_EDGE('',*,*,#2877,.F.);
#3762=ORIENTED_EDGE('',*,*,#2878,.F.);
#3763=ORIENTED_EDGE('',*,*,#2784,.F.);
#3764=ORIENTED_EDGE('',*,*,#2810,.T.);
#3765=ORIENTED_EDGE('',*,*,#2786,.T.);
#3766=ORIENTED_EDGE('',*,*,#2879,.T.);
#3767=ORIENTED_EDGE('',*,*,#2811,.F.);
#3768=ORIENTED_EDGE('',*,*,#2880,.F.);
#3769=ORIENTED_EDGE('',*,*,#2794,.F.);
#3770=ORIENTED_EDGE('',*,*,#2807,.T.);
#3771=ORIENTED_EDGE('',*,*,#2796,.T.);
#3772=ORIENTED_EDGE('',*,*,#2881,.T.);
#3773=ORIENTED_EDGE('',*,*,#2808,.F.);
#3774=ORIENTED_EDGE('',*,*,#2882,.F.);
#3775=ORIENTED_EDGE('',*,*,#2835,.F.);
#3776=ORIENTED_EDGE('',*,*,#2863,.T.);
#3777=ORIENTED_EDGE('',*,*,#2847,.T.);
#3778=ORIENTED_EDGE('',*,*,#2883,.F.);
#3779=ORIENTED_EDGE('',*,*,#2770,.T.);
#3780=ORIENTED_EDGE('',*,*,#2799,.F.);
#3781=ORIENTED_EDGE('',*,*,#2768,.F.);
#3782=ORIENTED_EDGE('',*,*,#2884,.F.);
#3783=ORIENTED_EDGE('',*,*,#2773,.T.);
#3784=ORIENTED_EDGE('',*,*,#2802,.F.);
#3785=ORIENTED_EDGE('',*,*,#2865,.F.);
#3786=ORIENTED_EDGE('',*,*,#2885,.F.);
#3787=ORIENTED_EDGE('',*,*,#2872,.F.);
#3788=ORIENTED_EDGE('',*,*,#2875,.T.);
#3789=ORIENTED_EDGE('',*,*,#2877,.T.);
#3790=ORIENTED_EDGE('',*,*,#2886,.F.);
#3791=ORIENTED_EDGE('',*,*,#2791,.T.);
#3792=ORIENTED_EDGE('',*,*,#2804,.F.);
#3793=ORIENTED_EDGE('',*,*,#2789,.F.);
#3794=ORIENTED_EDGE('',*,*,#2882,.T.);
#3795=ORIENTED_EDGE('',*,*,#2788,.T.);
#3796=ORIENTED_EDGE('',*,*,#2803,.T.);
#3797=ORIENTED_EDGE('',*,*,#2792,.F.);
#3798=ORIENTED_EDGE('',*,*,#2886,.T.);
#3799=ORIENTED_EDGE('',*,*,#2876,.F.);
#3800=ORIENTED_EDGE('',*,*,#2873,.F.);
#3801=ORIENTED_EDGE('',*,*,#2870,.T.);
#3802=ORIENTED_EDGE('',*,*,#2885,.T.);
#3803=ORIENTED_EDGE('',*,*,#2864,.T.);
#3804=ORIENTED_EDGE('',*,*,#2800,.T.);
#3805=ORIENTED_EDGE('',*,*,#2774,.F.);
#3806=ORIENTED_EDGE('',*,*,#2884,.T.);
#3807=ORIENTED_EDGE('',*,*,#2767,.T.);
#3808=ORIENTED_EDGE('',*,*,#2798,.T.);
#3809=ORIENTED_EDGE('',*,*,#2771,.F.);
#3810=ORIENTED_EDGE('',*,*,#2883,.T.);
#3811=ORIENTED_EDGE('',*,*,#2846,.T.);
#3812=ORIENTED_EDGE('',*,*,#2818,.T.);
#3813=ORIENTED_EDGE('',*,*,#2867,.F.);
#3814=ORIENTED_EDGE('',*,*,#2777,.F.);
#3815=ORIENTED_EDGE('',*,*,#2866,.T.);
#3816=ORIENTED_EDGE('',*,*,#2815,.F.);
#3817=ORIENTED_EDGE('',*,*,#2869,.F.);
#3818=ORIENTED_EDGE('',*,*,#2781,.F.);
#3819=ORIENTED_EDGE('',*,*,#2868,.T.);
#3820=ORIENTED_EDGE('',*,*,#2812,.F.);
#3821=ORIENTED_EDGE('',*,*,#2879,.F.);
#3822=ORIENTED_EDGE('',*,*,#2785,.F.);
#3823=ORIENTED_EDGE('',*,*,#2878,.T.);
#3824=ORIENTED_EDGE('',*,*,#2809,.F.);
#3825=ORIENTED_EDGE('',*,*,#2881,.F.);
#3826=ORIENTED_EDGE('',*,*,#2795,.F.);
#3827=ORIENTED_EDGE('',*,*,#2880,.T.);
#3828=ORIENTED_EDGE('',*,*,#2806,.F.);
#3829=ORIENTED_EDGE('',*,*,#2836,.F.);
#3830=ORIENTED_EDGE('',*,*,#2887,.T.);
#3831=ORIENTED_EDGE('',*,*,#2888,.T.);
#3832=ORIENTED_EDGE('',*,*,#2889,.F.);
#3833=ORIENTED_EDGE('',*,*,#2890,.T.);
#3834=ORIENTED_EDGE('',*,*,#2891,.T.);
#3835=ORIENTED_EDGE('',*,*,#2892,.T.);
#3836=ORIENTED_EDGE('',*,*,#2893,.F.);
#3837=ORIENTED_EDGE('',*,*,#2894,.T.);
#3838=ORIENTED_EDGE('',*,*,#2895,.T.);
#3839=ORIENTED_EDGE('',*,*,#2896,.T.);
#3840=ORIENTED_EDGE('',*,*,#2897,.F.);
#3841=ORIENTED_EDGE('',*,*,#2898,.F.);
#3842=ORIENTED_EDGE('',*,*,#2899,.T.);
#3843=ORIENTED_EDGE('',*,*,#2900,.T.);
#3844=ORIENTED_EDGE('',*,*,#2901,.F.);
#3845=ORIENTED_EDGE('',*,*,#2902,.F.);
#3846=ORIENTED_EDGE('',*,*,#2903,.T.);
#3847=ORIENTED_EDGE('',*,*,#2904,.T.);
#3848=ORIENTED_EDGE('',*,*,#2905,.F.);
#3849=ORIENTED_EDGE('',*,*,#2906,.F.);
#3850=ORIENTED_EDGE('',*,*,#2907,.T.);
#3851=ORIENTED_EDGE('',*,*,#2908,.T.);
#3852=ORIENTED_EDGE('',*,*,#2909,.F.);
#3853=ORIENTED_EDGE('',*,*,#2910,.F.);
#3854=ORIENTED_EDGE('',*,*,#2911,.T.);
#3855=ORIENTED_EDGE('',*,*,#2912,.T.);
#3856=ORIENTED_EDGE('',*,*,#2913,.F.);
#3857=ORIENTED_EDGE('',*,*,#2914,.T.);
#3858=ORIENTED_EDGE('',*,*,#2915,.T.);
#3859=ORIENTED_EDGE('',*,*,#2916,.T.);
#3860=ORIENTED_EDGE('',*,*,#2917,.F.);
#3861=ORIENTED_EDGE('',*,*,#2918,.F.);
#3862=ORIENTED_EDGE('',*,*,#2919,.T.);
#3863=ORIENTED_EDGE('',*,*,#2920,.T.);
#3864=ORIENTED_EDGE('',*,*,#2918,.T.);
#3865=ORIENTED_EDGE('',*,*,#2921,.T.);
#3866=ORIENTED_EDGE('',*,*,#2737,.F.);
#3867=ORIENTED_EDGE('',*,*,#2921,.F.);
#3868=ORIENTED_EDGE('',*,*,#2917,.T.);
#3869=ORIENTED_EDGE('',*,*,#2922,.T.);
#3870=ORIENTED_EDGE('',*,*,#2738,.F.);
#3871=ORIENTED_EDGE('',*,*,#2916,.F.);
#3872=ORIENTED_EDGE('',*,*,#2923,.T.);
#3873=ORIENTED_EDGE('',*,*,#2924,.T.);
#3874=ORIENTED_EDGE('',*,*,#2735,.T.);
#3875=ORIENTED_EDGE('',*,*,#2922,.F.);
#3876=ORIENTED_EDGE('',*,*,#2914,.F.);
#3877=ORIENTED_EDGE('',*,*,#2925,.T.);
#3878=ORIENTED_EDGE('',*,*,#2741,.T.);
#3879=ORIENTED_EDGE('',*,*,#2926,.F.);
#3880=ORIENTED_EDGE('',*,*,#2925,.F.);
#3881=ORIENTED_EDGE('',*,*,#2913,.T.);
#3882=ORIENTED_EDGE('',*,*,#2927,.T.);
#3883=ORIENTED_EDGE('',*,*,#2928,.T.);
#3884=ORIENTED_EDGE('',*,*,#2742,.F.);
#3885=ORIENTED_EDGE('',*,*,#2911,.F.);
#3886=ORIENTED_EDGE('',*,*,#2926,.T.);
#3887=ORIENTED_EDGE('',*,*,#2740,.T.);
#3888=ORIENTED_EDGE('',*,*,#2929,.T.);
#3889=ORIENTED_EDGE('',*,*,#2930,.T.);
#3890=ORIENTED_EDGE('',*,*,#2931,.T.);
#3891=ORIENTED_EDGE('',*,*,#2932,.T.);
#3892=ORIENTED_EDGE('',*,*,#2910,.T.);
#3893=ORIENTED_EDGE('',*,*,#2933,.T.);
#3894=ORIENTED_EDGE('',*,*,#2765,.F.);
#3895=ORIENTED_EDGE('',*,*,#2933,.F.);
#3896=ORIENTED_EDGE('',*,*,#2909,.T.);
#3897=ORIENTED_EDGE('',*,*,#2934,.T.);
#3898=ORIENTED_EDGE('',*,*,#2766,.F.);
#3899=ORIENTED_EDGE('',*,*,#2908,.F.);
#3900=ORIENTED_EDGE('',*,*,#2935,.T.);
#3901=ORIENTED_EDGE('',*,*,#2936,.T.);
#3902=ORIENTED_EDGE('',*,*,#2763,.T.);
#3903=ORIENTED_EDGE('',*,*,#2934,.F.);
#3904=ORIENTED_EDGE('',*,*,#2937,.T.);
#3905=ORIENTED_EDGE('',*,*,#2938,.T.);
#3906=ORIENTED_EDGE('',*,*,#2906,.T.);
#3907=ORIENTED_EDGE('',*,*,#2939,.T.);
#3908=ORIENTED_EDGE('',*,*,#2745,.F.);
#3909=ORIENTED_EDGE('',*,*,#2939,.F.);
#3910=ORIENTED_EDGE('',*,*,#2905,.T.);
#3911=ORIENTED_EDGE('',*,*,#2940,.T.);
#3912=ORIENTED_EDGE('',*,*,#2746,.F.);
#3913=ORIENTED_EDGE('',*,*,#2904,.F.);
#3914=ORIENTED_EDGE('',*,*,#2941,.T.);
#3915=ORIENTED_EDGE('',*,*,#2942,.T.);
#3916=ORIENTED_EDGE('',*,*,#2743,.T.);
#3917=ORIENTED_EDGE('',*,*,#2940,.F.);
#3918=ORIENTED_EDGE('',*,*,#2943,.T.);
#3919=ORIENTED_EDGE('',*,*,#2944,.T.);
#3920=ORIENTED_EDGE('',*,*,#2902,.T.);
#3921=ORIENTED_EDGE('',*,*,#2945,.T.);
#3922=ORIENTED_EDGE('',*,*,#2761,.F.);
#3923=ORIENTED_EDGE('',*,*,#2945,.F.);
#3924=ORIENTED_EDGE('',*,*,#2901,.T.);
#3925=ORIENTED_EDGE('',*,*,#2946,.T.);
#3926=ORIENTED_EDGE('',*,*,#2762,.F.);
#3927=ORIENTED_EDGE('',*,*,#2900,.F.);
#3928=ORIENTED_EDGE('',*,*,#2947,.T.);
#3929=ORIENTED_EDGE('',*,*,#2948,.T.);
#3930=ORIENTED_EDGE('',*,*,#2759,.T.);
#3931=ORIENTED_EDGE('',*,*,#2946,.F.);
#3932=ORIENTED_EDGE('',*,*,#2949,.T.);
#3933=ORIENTED_EDGE('',*,*,#2950,.T.);
#3934=ORIENTED_EDGE('',*,*,#2898,.T.);
#3935=ORIENTED_EDGE('',*,*,#2951,.T.);
#3936=ORIENTED_EDGE('',*,*,#2757,.F.);
#3937=ORIENTED_EDGE('',*,*,#2951,.F.);
#3938=ORIENTED_EDGE('',*,*,#2897,.T.);
#3939=ORIENTED_EDGE('',*,*,#2952,.T.);
#3940=ORIENTED_EDGE('',*,*,#2758,.F.);
#3941=ORIENTED_EDGE('',*,*,#2896,.F.);
#3942=ORIENTED_EDGE('',*,*,#2953,.T.);
#3943=ORIENTED_EDGE('',*,*,#2954,.T.);
#3944=ORIENTED_EDGE('',*,*,#2755,.T.);
#3945=ORIENTED_EDGE('',*,*,#2952,.F.);
#3946=ORIENTED_EDGE('',*,*,#2894,.F.);
#3947=ORIENTED_EDGE('',*,*,#2955,.T.);
#3948=ORIENTED_EDGE('',*,*,#2749,.T.);
#3949=ORIENTED_EDGE('',*,*,#2956,.F.);
#3950=ORIENTED_EDGE('',*,*,#2955,.F.);
#3951=ORIENTED_EDGE('',*,*,#2893,.T.);
#3952=ORIENTED_EDGE('',*,*,#2957,.T.);
#3953=ORIENTED_EDGE('',*,*,#2958,.T.);
#3954=ORIENTED_EDGE('',*,*,#2750,.F.);
#3955=ORIENTED_EDGE('',*,*,#2891,.F.);
#3956=ORIENTED_EDGE('',*,*,#2956,.T.);
#3957=ORIENTED_EDGE('',*,*,#2748,.T.);
#3958=ORIENTED_EDGE('',*,*,#2959,.T.);
#3959=ORIENTED_EDGE('',*,*,#2960,.T.);
#3960=ORIENTED_EDGE('',*,*,#2890,.F.);
#3961=ORIENTED_EDGE('',*,*,#2961,.T.);
#3962=ORIENTED_EDGE('',*,*,#2753,.T.);
#3963=ORIENTED_EDGE('',*,*,#2962,.F.);
#3964=ORIENTED_EDGE('',*,*,#2961,.F.);
#3965=ORIENTED_EDGE('',*,*,#2889,.T.);
#3966=ORIENTED_EDGE('',*,*,#2963,.T.);
#3967=ORIENTED_EDGE('',*,*,#2964,.T.);
#3968=ORIENTED_EDGE('',*,*,#2754,.F.);
#3969=ORIENTED_EDGE('',*,*,#2887,.F.);
#3970=ORIENTED_EDGE('',*,*,#2962,.T.);
#3971=ORIENTED_EDGE('',*,*,#2752,.T.);
#3972=ORIENTED_EDGE('',*,*,#2965,.T.);
#3973=ORIENTED_EDGE('',*,*,#2966,.T.);
#3974=ORIENTED_EDGE('',*,*,#2907,.F.);
#3975=ORIENTED_EDGE('',*,*,#2932,.F.);
#3976=ORIENTED_EDGE('',*,*,#2967,.F.);
#3977=ORIENTED_EDGE('',*,*,#2935,.F.);
#3978=ORIENTED_EDGE('',*,*,#2931,.F.);
#3979=ORIENTED_EDGE('',*,*,#2764,.F.);
#3980=ORIENTED_EDGE('',*,*,#2936,.F.);
#3981=ORIENTED_EDGE('',*,*,#2967,.T.);
#3982=ORIENTED_EDGE('',*,*,#2899,.F.);
#3983=ORIENTED_EDGE('',*,*,#2944,.F.);
#3984=ORIENTED_EDGE('',*,*,#2968,.F.);
#3985=ORIENTED_EDGE('',*,*,#2947,.F.);
#3986=ORIENTED_EDGE('',*,*,#2943,.F.);
#3987=ORIENTED_EDGE('',*,*,#2760,.F.);
#3988=ORIENTED_EDGE('',*,*,#2948,.F.);
#3989=ORIENTED_EDGE('',*,*,#2968,.T.);
#3990=ORIENTED_EDGE('',*,*,#2895,.F.);
#3991=ORIENTED_EDGE('',*,*,#2950,.F.);
#3992=ORIENTED_EDGE('',*,*,#2969,.F.);
#3993=ORIENTED_EDGE('',*,*,#2953,.F.);
#3994=ORIENTED_EDGE('',*,*,#2949,.F.);
#3995=ORIENTED_EDGE('',*,*,#2756,.F.);
#3996=ORIENTED_EDGE('',*,*,#2954,.F.);
#3997=ORIENTED_EDGE('',*,*,#2969,.T.);
#3998=ORIENTED_EDGE('',*,*,#2970,.F.);
#3999=ORIENTED_EDGE('',*,*,#2963,.F.);
#4000=ORIENTED_EDGE('',*,*,#2888,.F.);
#4001=ORIENTED_EDGE('',*,*,#2966,.F.);
#4002=ORIENTED_EDGE('',*,*,#2964,.F.);
#4003=ORIENTED_EDGE('',*,*,#2970,.T.);
#4004=ORIENTED_EDGE('',*,*,#2965,.F.);
#4005=ORIENTED_EDGE('',*,*,#2751,.F.);
#4006=ORIENTED_EDGE('',*,*,#2971,.F.);
#4007=ORIENTED_EDGE('',*,*,#2957,.F.);
#4008=ORIENTED_EDGE('',*,*,#2892,.F.);
#4009=ORIENTED_EDGE('',*,*,#2960,.F.);
#4010=ORIENTED_EDGE('',*,*,#2958,.F.);
#4011=ORIENTED_EDGE('',*,*,#2971,.T.);
#4012=ORIENTED_EDGE('',*,*,#2959,.F.);
#4013=ORIENTED_EDGE('',*,*,#2747,.F.);
#4014=ORIENTED_EDGE('',*,*,#2903,.F.);
#4015=ORIENTED_EDGE('',*,*,#2938,.F.);
#4016=ORIENTED_EDGE('',*,*,#2972,.F.);
#4017=ORIENTED_EDGE('',*,*,#2941,.F.);
#4018=ORIENTED_EDGE('',*,*,#2937,.F.);
#4019=ORIENTED_EDGE('',*,*,#2744,.F.);
#4020=ORIENTED_EDGE('',*,*,#2942,.F.);
#4021=ORIENTED_EDGE('',*,*,#2972,.T.);
#4022=ORIENTED_EDGE('',*,*,#2973,.F.);
#4023=ORIENTED_EDGE('',*,*,#2927,.F.);
#4024=ORIENTED_EDGE('',*,*,#2912,.F.);
#4025=ORIENTED_EDGE('',*,*,#2930,.F.);
#4026=ORIENTED_EDGE('',*,*,#2928,.F.);
#4027=ORIENTED_EDGE('',*,*,#2973,.T.);
#4028=ORIENTED_EDGE('',*,*,#2929,.F.);
#4029=ORIENTED_EDGE('',*,*,#2739,.F.);
#4030=ORIENTED_EDGE('',*,*,#2915,.F.);
#4031=ORIENTED_EDGE('',*,*,#2920,.F.);
#4032=ORIENTED_EDGE('',*,*,#2974,.F.);
#4033=ORIENTED_EDGE('',*,*,#2923,.F.);
#4034=ORIENTED_EDGE('',*,*,#2919,.F.);
#4035=ORIENTED_EDGE('',*,*,#2736,.F.);
#4036=ORIENTED_EDGE('',*,*,#2924,.F.);
#4037=ORIENTED_EDGE('',*,*,#2974,.T.);
#4038=ORIENTED_EDGE('',*,*,#2975,.F.);
#4039=ORIENTED_EDGE('',*,*,#2976,.F.);
#4040=ORIENTED_EDGE('',*,*,#2977,.T.);
#4041=ORIENTED_EDGE('',*,*,#2976,.T.);
#4042=ORIENTED_EDGE('',*,*,#2978,.T.);
#4043=ORIENTED_EDGE('',*,*,#2979,.F.);
#4044=ORIENTED_EDGE('',*,*,#2980,.F.);
#4045=ORIENTED_EDGE('',*,*,#2979,.T.);
#4046=ORIENTED_EDGE('',*,*,#2981,.T.);
#4047=ORIENTED_EDGE('',*,*,#2982,.F.);
#4048=ORIENTED_EDGE('',*,*,#2702,.T.);
#4049=ORIENTED_EDGE('',*,*,#2983,.T.);
#4050=ORIENTED_EDGE('',*,*,#2984,.F.);
#4051=ORIENTED_EDGE('',*,*,#2985,.F.);
#4052=ORIENTED_EDGE('',*,*,#2984,.T.);
#4053=ORIENTED_EDGE('',*,*,#2986,.T.);
#4054=ORIENTED_EDGE('',*,*,#2987,.F.);
#4055=ORIENTED_EDGE('',*,*,#2708,.T.);
#4056=ORIENTED_EDGE('',*,*,#2988,.T.);
#4057=ORIENTED_EDGE('',*,*,#2725,.F.);
#4058=ORIENTED_EDGE('',*,*,#2989,.F.);
#4059=ORIENTED_EDGE('',*,*,#2990,.F.);
#4060=ORIENTED_EDGE('',*,*,#2991,.T.);
#4061=ORIENTED_EDGE('',*,*,#2990,.T.);
#4062=ORIENTED_EDGE('',*,*,#2992,.T.);
#4063=ORIENTED_EDGE('',*,*,#2710,.F.);
#4064=ORIENTED_EDGE('',*,*,#2993,.F.);
#4065=ORIENTED_EDGE('',*,*,#2994,.F.);
#4066=ORIENTED_EDGE('',*,*,#2995,.F.);
#4067=ORIENTED_EDGE('',*,*,#2996,.T.);
#4068=ORIENTED_EDGE('',*,*,#2995,.T.);
#4069=ORIENTED_EDGE('',*,*,#2997,.T.);
#4070=ORIENTED_EDGE('',*,*,#2998,.F.);
#4071=ORIENTED_EDGE('',*,*,#2999,.F.);
#4072=ORIENTED_EDGE('',*,*,#2998,.T.);
#4073=ORIENTED_EDGE('',*,*,#3000,.T.);
#4074=ORIENTED_EDGE('',*,*,#3001,.F.);
#4075=ORIENTED_EDGE('',*,*,#3002,.F.);
#4076=ORIENTED_EDGE('',*,*,#2697,.F.);
#4077=ORIENTED_EDGE('',*,*,#2723,.T.);
#4078=ORIENTED_EDGE('',*,*,#2700,.T.);
#4079=ORIENTED_EDGE('',*,*,#3003,.F.);
#4080=ORIENTED_EDGE('',*,*,#2715,.F.);
#4081=ORIENTED_EDGE('',*,*,#2727,.T.);
#4082=ORIENTED_EDGE('',*,*,#2718,.T.);
#4083=ORIENTED_EDGE('',*,*,#3004,.F.);
#4084=ORIENTED_EDGE('',*,*,#2691,.F.);
#4085=ORIENTED_EDGE('',*,*,#2721,.T.);
#4086=ORIENTED_EDGE('',*,*,#2694,.T.);
#4087=ORIENTED_EDGE('',*,*,#3005,.F.);
#4088=ORIENTED_EDGE('',*,*,#2844,.F.);
#4089=ORIENTED_EDGE('',*,*,#2652,.F.);
#4090=ORIENTED_EDGE('',*,*,#2829,.T.);
#4091=ORIENTED_EDGE('',*,*,#3006,.F.);
#4092=ORIENTED_EDGE('',*,*,#2996,.F.);
#4093=ORIENTED_EDGE('',*,*,#2999,.T.);
#4094=ORIENTED_EDGE('',*,*,#3001,.T.);
#4095=ORIENTED_EDGE('',*,*,#3007,.F.);
#4096=ORIENTED_EDGE('',*,*,#2991,.F.);
#4097=ORIENTED_EDGE('',*,*,#2993,.T.);
#4098=ORIENTED_EDGE('',*,*,#2712,.T.);
#4099=ORIENTED_EDGE('',*,*,#3008,.F.);
#4100=ORIENTED_EDGE('',*,*,#2703,.F.);
#4101=ORIENTED_EDGE('',*,*,#2985,.T.);
#4102=ORIENTED_EDGE('',*,*,#2987,.T.);
#4103=ORIENTED_EDGE('',*,*,#3009,.F.);
#4104=ORIENTED_EDGE('',*,*,#2977,.F.);
#4105=ORIENTED_EDGE('',*,*,#2980,.T.);
#4106=ORIENTED_EDGE('',*,*,#2982,.T.);
#4107=ORIENTED_EDGE('',*,*,#2845,.T.);
#4108=ORIENTED_EDGE('',*,*,#3005,.T.);
#4109=ORIENTED_EDGE('',*,*,#2981,.F.);
#4110=ORIENTED_EDGE('',*,*,#2978,.F.);
#4111=ORIENTED_EDGE('',*,*,#2975,.T.);
#4112=ORIENTED_EDGE('',*,*,#3009,.T.);
#4113=ORIENTED_EDGE('',*,*,#2986,.F.);
#4114=ORIENTED_EDGE('',*,*,#2983,.F.);
#4115=ORIENTED_EDGE('',*,*,#2701,.T.);
#4116=ORIENTED_EDGE('',*,*,#3008,.T.);
#4117=ORIENTED_EDGE('',*,*,#2711,.F.);
#4118=ORIENTED_EDGE('',*,*,#2992,.F.);
#4119=ORIENTED_EDGE('',*,*,#2989,.T.);
#4120=ORIENTED_EDGE('',*,*,#3007,.T.);
#4121=ORIENTED_EDGE('',*,*,#3000,.F.);
#4122=ORIENTED_EDGE('',*,*,#2997,.F.);
#4123=ORIENTED_EDGE('',*,*,#2994,.T.);
#4124=ORIENTED_EDGE('',*,*,#3006,.T.);
#4125=ORIENTED_EDGE('',*,*,#2828,.T.);
#4126=ORIENTED_EDGE('',*,*,#2728,.T.);
#4127=ORIENTED_EDGE('',*,*,#2713,.T.);
#4128=ORIENTED_EDGE('',*,*,#3003,.T.);
#4129=ORIENTED_EDGE('',*,*,#2717,.F.);
#4130=ORIENTED_EDGE('',*,*,#2726,.F.);
#4131=ORIENTED_EDGE('',*,*,#2988,.F.);
#4132=ORIENTED_EDGE('',*,*,#2707,.F.);
#4133=ORIENTED_EDGE('',*,*,#2704,.T.);
#4134=ORIENTED_EDGE('',*,*,#2724,.F.);
#4135=ORIENTED_EDGE('',*,*,#2695,.T.);
#4136=ORIENTED_EDGE('',*,*,#3002,.T.);
#4137=ORIENTED_EDGE('',*,*,#2699,.F.);
#4138=ORIENTED_EDGE('',*,*,#2722,.F.);
#4139=ORIENTED_EDGE('',*,*,#2689,.T.);
#4140=ORIENTED_EDGE('',*,*,#3004,.T.);
#4141=ORIENTED_EDGE('',*,*,#2693,.F.);
#4142=ORIENTED_EDGE('',*,*,#2720,.F.);
#4143=ORIENTED_EDGE('',*,*,#3010,.T.);
#4144=ORIENTED_EDGE('',*,*,#3011,.T.);
#4145=ORIENTED_EDGE('',*,*,#3012,.F.);
#4146=ORIENTED_EDGE('',*,*,#3013,.T.);
#4147=ORIENTED_EDGE('',*,*,#3014,.T.);
#4148=ORIENTED_EDGE('',*,*,#3015,.T.);
#4149=ORIENTED_EDGE('',*,*,#3016,.F.);
#4150=ORIENTED_EDGE('',*,*,#3017,.F.);
#4151=ORIENTED_EDGE('',*,*,#3018,.T.);
#4152=ORIENTED_EDGE('',*,*,#3019,.T.);
#4153=ORIENTED_EDGE('',*,*,#3020,.F.);
#4154=ORIENTED_EDGE('',*,*,#3021,.F.);
#4155=ORIENTED_EDGE('',*,*,#3022,.T.);
#4156=ORIENTED_EDGE('',*,*,#3023,.T.);
#4157=ORIENTED_EDGE('',*,*,#3024,.F.);
#4158=ORIENTED_EDGE('',*,*,#3025,.F.);
#4159=ORIENTED_EDGE('',*,*,#3026,.T.);
#4160=ORIENTED_EDGE('',*,*,#3027,.T.);
#4161=ORIENTED_EDGE('',*,*,#3028,.F.);
#4162=ORIENTED_EDGE('',*,*,#3029,.F.);
#4163=ORIENTED_EDGE('',*,*,#3030,.T.);
#4164=ORIENTED_EDGE('',*,*,#3031,.T.);
#4165=ORIENTED_EDGE('',*,*,#3032,.F.);
#4166=ORIENTED_EDGE('',*,*,#3033,.T.);
#4167=ORIENTED_EDGE('',*,*,#3034,.T.);
#4168=ORIENTED_EDGE('',*,*,#3035,.T.);
#4169=ORIENTED_EDGE('',*,*,#3036,.F.);
#4170=ORIENTED_EDGE('',*,*,#3037,.F.);
#4171=ORIENTED_EDGE('',*,*,#3038,.T.);
#4172=ORIENTED_EDGE('',*,*,#3039,.T.);
#4173=ORIENTED_EDGE('',*,*,#3040,.F.);
#4174=ORIENTED_EDGE('',*,*,#3041,.T.);
#4175=ORIENTED_EDGE('',*,*,#3041,.F.);
#4176=ORIENTED_EDGE('',*,*,#3042,.T.);
#4177=ORIENTED_EDGE('',*,*,#2680,.F.);
#4178=ORIENTED_EDGE('',*,*,#3043,.F.);
#4179=ORIENTED_EDGE('',*,*,#3042,.F.);
#4180=ORIENTED_EDGE('',*,*,#3040,.T.);
#4181=ORIENTED_EDGE('',*,*,#3044,.T.);
#4182=ORIENTED_EDGE('',*,*,#3045,.T.);
#4183=ORIENTED_EDGE('',*,*,#3046,.T.);
#4184=ORIENTED_EDGE('',*,*,#2677,.T.);
#4185=ORIENTED_EDGE('',*,*,#3047,.T.);
#4186=ORIENTED_EDGE('',*,*,#3048,.T.);
#4187=ORIENTED_EDGE('',*,*,#3045,.F.);
#4188=ORIENTED_EDGE('',*,*,#3049,.T.);
#4189=ORIENTED_EDGE('',*,*,#3038,.F.);
#4190=ORIENTED_EDGE('',*,*,#3043,.T.);
#4191=ORIENTED_EDGE('',*,*,#2679,.F.);
#4192=ORIENTED_EDGE('',*,*,#3050,.T.);
#4193=ORIENTED_EDGE('',*,*,#3047,.F.);
#4194=ORIENTED_EDGE('',*,*,#3051,.T.);
#4195=ORIENTED_EDGE('',*,*,#3052,.T.);
#4196=ORIENTED_EDGE('',*,*,#3053,.T.);
#4197=ORIENTED_EDGE('',*,*,#3054,.F.);
#4198=ORIENTED_EDGE('',*,*,#3055,.T.);
#4199=ORIENTED_EDGE('',*,*,#3052,.F.);
#4200=ORIENTED_EDGE('',*,*,#3056,.T.);
#4201=ORIENTED_EDGE('',*,*,#3037,.T.);
#4202=ORIENTED_EDGE('',*,*,#3057,.T.);
#4203=ORIENTED_EDGE('',*,*,#2686,.T.);
#4204=ORIENTED_EDGE('',*,*,#3058,.T.);
#4205=ORIENTED_EDGE('',*,*,#3057,.F.);
#4206=ORIENTED_EDGE('',*,*,#3036,.T.);
#4207=ORIENTED_EDGE('',*,*,#3059,.T.);
#4208=ORIENTED_EDGE('',*,*,#2687,.T.);
#4209=ORIENTED_EDGE('',*,*,#3035,.F.);
#4210=ORIENTED_EDGE('',*,*,#3060,.T.);
#4211=ORIENTED_EDGE('',*,*,#3054,.T.);
#4212=ORIENTED_EDGE('',*,*,#3061,.T.);
#4213=ORIENTED_EDGE('',*,*,#2688,.F.);
#4214=ORIENTED_EDGE('',*,*,#3059,.F.);
#4215=ORIENTED_EDGE('',*,*,#3033,.F.);
#4216=ORIENTED_EDGE('',*,*,#3062,.T.);
#4217=ORIENTED_EDGE('',*,*,#2660,.F.);
#4218=ORIENTED_EDGE('',*,*,#3063,.F.);
#4219=ORIENTED_EDGE('',*,*,#3062,.F.);
#4220=ORIENTED_EDGE('',*,*,#3032,.T.);
#4221=ORIENTED_EDGE('',*,*,#3064,.T.);
#4222=ORIENTED_EDGE('',*,*,#3065,.T.);
#4223=ORIENTED_EDGE('',*,*,#3066,.T.);
#4224=ORIENTED_EDGE('',*,*,#2657,.T.);
#4225=ORIENTED_EDGE('',*,*,#3067,.T.);
#4226=ORIENTED_EDGE('',*,*,#3068,.T.);
#4227=ORIENTED_EDGE('',*,*,#3065,.F.);
#4228=ORIENTED_EDGE('',*,*,#3069,.T.);
#4229=ORIENTED_EDGE('',*,*,#3030,.F.);
#4230=ORIENTED_EDGE('',*,*,#3063,.T.);
#4231=ORIENTED_EDGE('',*,*,#2659,.F.);
#4232=ORIENTED_EDGE('',*,*,#3070,.T.);
#4233=ORIENTED_EDGE('',*,*,#3067,.F.);
#4234=ORIENTED_EDGE('',*,*,#3071,.T.);
#4235=ORIENTED_EDGE('',*,*,#3072,.T.);
#4236=ORIENTED_EDGE('',*,*,#3073,.T.);
#4237=ORIENTED_EDGE('',*,*,#3074,.F.);
#4238=ORIENTED_EDGE('',*,*,#3075,.T.);
#4239=ORIENTED_EDGE('',*,*,#3072,.F.);
#4240=ORIENTED_EDGE('',*,*,#3076,.T.);
#4241=ORIENTED_EDGE('',*,*,#3029,.T.);
#4242=ORIENTED_EDGE('',*,*,#3077,.T.);
#4243=ORIENTED_EDGE('',*,*,#2670,.T.);
#4244=ORIENTED_EDGE('',*,*,#3078,.T.);
#4245=ORIENTED_EDGE('',*,*,#3077,.F.);
#4246=ORIENTED_EDGE('',*,*,#3028,.T.);
#4247=ORIENTED_EDGE('',*,*,#3079,.T.);
#4248=ORIENTED_EDGE('',*,*,#2671,.T.);
#4249=ORIENTED_EDGE('',*,*,#3027,.F.);
#4250=ORIENTED_EDGE('',*,*,#3080,.T.);
#4251=ORIENTED_EDGE('',*,*,#3074,.T.);
#4252=ORIENTED_EDGE('',*,*,#3081,.T.);
#4253=ORIENTED_EDGE('',*,*,#2672,.F.);
#4254=ORIENTED_EDGE('',*,*,#3079,.F.);
#4255=ORIENTED_EDGE('',*,*,#3082,.T.);
#4256=ORIENTED_EDGE('',*,*,#3083,.T.);
#4257=ORIENTED_EDGE('',*,*,#3084,.F.);
#4258=ORIENTED_EDGE('',*,*,#3085,.T.);
#4259=ORIENTED_EDGE('',*,*,#3082,.F.);
#4260=ORIENTED_EDGE('',*,*,#3086,.T.);
#4261=ORIENTED_EDGE('',*,*,#3025,.T.);
#4262=ORIENTED_EDGE('',*,*,#3087,.T.);
#4263=ORIENTED_EDGE('',*,*,#2682,.T.);
#4264=ORIENTED_EDGE('',*,*,#3088,.T.);
#4265=ORIENTED_EDGE('',*,*,#3087,.F.);
#4266=ORIENTED_EDGE('',*,*,#3024,.T.);
#4267=ORIENTED_EDGE('',*,*,#3089,.T.);
#4268=ORIENTED_EDGE('',*,*,#2683,.T.);
#4269=ORIENTED_EDGE('',*,*,#3023,.F.);
#4270=ORIENTED_EDGE('',*,*,#3090,.T.);
#4271=ORIENTED_EDGE('',*,*,#3084,.T.);
#4272=ORIENTED_EDGE('',*,*,#3091,.T.);
#4273=ORIENTED_EDGE('',*,*,#2684,.F.);
#4274=ORIENTED_EDGE('',*,*,#3089,.F.);
#4275=ORIENTED_EDGE('',*,*,#3092,.T.);
#4276=ORIENTED_EDGE('',*,*,#3093,.T.);
#4277=ORIENTED_EDGE('',*,*,#3094,.F.);
#4278=ORIENTED_EDGE('',*,*,#3095,.T.);
#4279=ORIENTED_EDGE('',*,*,#3092,.F.);
#4280=ORIENTED_EDGE('',*,*,#3096,.T.);
#4281=ORIENTED_EDGE('',*,*,#3021,.T.);
#4282=ORIENTED_EDGE('',*,*,#3097,.T.);
#4283=ORIENTED_EDGE('',*,*,#2674,.T.);
#4284=ORIENTED_EDGE('',*,*,#3098,.T.);
#4285=ORIENTED_EDGE('',*,*,#3097,.F.);
#4286=ORIENTED_EDGE('',*,*,#3020,.T.);
#4287=ORIENTED_EDGE('',*,*,#3099,.T.);
#4288=ORIENTED_EDGE('',*,*,#2675,.T.);
#4289=ORIENTED_EDGE('',*,*,#3019,.F.);
#4290=ORIENTED_EDGE('',*,*,#3100,.T.);
#4291=ORIENTED_EDGE('',*,*,#3094,.T.);
#4292=ORIENTED_EDGE('',*,*,#3101,.T.);
#4293=ORIENTED_EDGE('',*,*,#2676,.F.);
#4294=ORIENTED_EDGE('',*,*,#3099,.F.);
#4295=ORIENTED_EDGE('',*,*,#3102,.T.);
#4296=ORIENTED_EDGE('',*,*,#3103,.T.);
#4297=ORIENTED_EDGE('',*,*,#3104,.F.);
#4298=ORIENTED_EDGE('',*,*,#3105,.T.);
#4299=ORIENTED_EDGE('',*,*,#3102,.F.);
#4300=ORIENTED_EDGE('',*,*,#3106,.T.);
#4301=ORIENTED_EDGE('',*,*,#3017,.T.);
#4302=ORIENTED_EDGE('',*,*,#3107,.T.);
#4303=ORIENTED_EDGE('',*,*,#2666,.T.);
#4304=ORIENTED_EDGE('',*,*,#3108,.T.);
#4305=ORIENTED_EDGE('',*,*,#3107,.F.);
#4306=ORIENTED_EDGE('',*,*,#3016,.T.);
#4307=ORIENTED_EDGE('',*,*,#3109,.T.);
#4308=ORIENTED_EDGE('',*,*,#2667,.T.);
#4309=ORIENTED_EDGE('',*,*,#3015,.F.);
#4310=ORIENTED_EDGE('',*,*,#3110,.T.);
#4311=ORIENTED_EDGE('',*,*,#3104,.T.);
#4312=ORIENTED_EDGE('',*,*,#3111,.T.);
#4313=ORIENTED_EDGE('',*,*,#2668,.F.);
#4314=ORIENTED_EDGE('',*,*,#3109,.F.);
#4315=ORIENTED_EDGE('',*,*,#3013,.F.);
#4316=ORIENTED_EDGE('',*,*,#3112,.T.);
#4317=ORIENTED_EDGE('',*,*,#2664,.F.);
#4318=ORIENTED_EDGE('',*,*,#3113,.F.);
#4319=ORIENTED_EDGE('',*,*,#3112,.F.);
#4320=ORIENTED_EDGE('',*,*,#3012,.T.);
#4321=ORIENTED_EDGE('',*,*,#3114,.T.);
#4322=ORIENTED_EDGE('',*,*,#3115,.T.);
#4323=ORIENTED_EDGE('',*,*,#3116,.T.);
#4324=ORIENTED_EDGE('',*,*,#2661,.T.);
#4325=ORIENTED_EDGE('',*,*,#3117,.T.);
#4326=ORIENTED_EDGE('',*,*,#3118,.T.);
#4327=ORIENTED_EDGE('',*,*,#3115,.F.);
#4328=ORIENTED_EDGE('',*,*,#3119,.T.);
#4329=ORIENTED_EDGE('',*,*,#3010,.F.);
#4330=ORIENTED_EDGE('',*,*,#3113,.T.);
#4331=ORIENTED_EDGE('',*,*,#2663,.F.);
#4332=ORIENTED_EDGE('',*,*,#3120,.T.);
#4333=ORIENTED_EDGE('',*,*,#3117,.F.);
#4334=ORIENTED_EDGE('',*,*,#3121,.T.);
#4335=ORIENTED_EDGE('',*,*,#3070,.F.);
#4336=ORIENTED_EDGE('',*,*,#2658,.F.);
#4337=ORIENTED_EDGE('',*,*,#3066,.F.);
#4338=ORIENTED_EDGE('',*,*,#3068,.F.);
#4339=ORIENTED_EDGE('',*,*,#3091,.F.);
#4340=ORIENTED_EDGE('',*,*,#3083,.F.);
#4341=ORIENTED_EDGE('',*,*,#3088,.F.);
#4342=ORIENTED_EDGE('',*,*,#2681,.F.);
#4343=ORIENTED_EDGE('',*,*,#3120,.F.);
#4344=ORIENTED_EDGE('',*,*,#2662,.F.);
#4345=ORIENTED_EDGE('',*,*,#3116,.F.);
#4346=ORIENTED_EDGE('',*,*,#3118,.F.);
#4347=ORIENTED_EDGE('',*,*,#3050,.F.);
#4348=ORIENTED_EDGE('',*,*,#2678,.F.);
#4349=ORIENTED_EDGE('',*,*,#3046,.F.);
#4350=ORIENTED_EDGE('',*,*,#3048,.F.);
#4351=ORIENTED_EDGE('',*,*,#3111,.F.);
#4352=ORIENTED_EDGE('',*,*,#3103,.F.);
#4353=ORIENTED_EDGE('',*,*,#3108,.F.);
#4354=ORIENTED_EDGE('',*,*,#2665,.F.);
#4355=ORIENTED_EDGE('',*,*,#3101,.F.);
#4356=ORIENTED_EDGE('',*,*,#3093,.F.);
#4357=ORIENTED_EDGE('',*,*,#3098,.F.);
#4358=ORIENTED_EDGE('',*,*,#2673,.F.);
#4359=ORIENTED_EDGE('',*,*,#3081,.F.);
#4360=ORIENTED_EDGE('',*,*,#3073,.F.);
#4361=ORIENTED_EDGE('',*,*,#3078,.F.);
#4362=ORIENTED_EDGE('',*,*,#2669,.F.);
#4363=ORIENTED_EDGE('',*,*,#3061,.F.);
#4364=ORIENTED_EDGE('',*,*,#3053,.F.);
#4365=ORIENTED_EDGE('',*,*,#3058,.F.);
#4366=ORIENTED_EDGE('',*,*,#2685,.F.);
#4367=ORIENTED_EDGE('',*,*,#3114,.F.);
#4368=ORIENTED_EDGE('',*,*,#3011,.F.);
#4369=ORIENTED_EDGE('',*,*,#3121,.F.);
#4370=ORIENTED_EDGE('',*,*,#3119,.F.);
#4371=ORIENTED_EDGE('',*,*,#3106,.F.);
#4372=ORIENTED_EDGE('',*,*,#3105,.F.);
#4373=ORIENTED_EDGE('',*,*,#3110,.F.);
#4374=ORIENTED_EDGE('',*,*,#3014,.F.);
#4375=ORIENTED_EDGE('',*,*,#3096,.F.);
#4376=ORIENTED_EDGE('',*,*,#3095,.F.);
#4377=ORIENTED_EDGE('',*,*,#3100,.F.);
#4378=ORIENTED_EDGE('',*,*,#3018,.F.);
#4379=ORIENTED_EDGE('',*,*,#3086,.F.);
#4380=ORIENTED_EDGE('',*,*,#3085,.F.);
#4381=ORIENTED_EDGE('',*,*,#3090,.F.);
#4382=ORIENTED_EDGE('',*,*,#3022,.F.);
#4383=ORIENTED_EDGE('',*,*,#3076,.F.);
#4384=ORIENTED_EDGE('',*,*,#3075,.F.);
#4385=ORIENTED_EDGE('',*,*,#3080,.F.);
#4386=ORIENTED_EDGE('',*,*,#3026,.F.);
#4387=ORIENTED_EDGE('',*,*,#3064,.F.);
#4388=ORIENTED_EDGE('',*,*,#3031,.F.);
#4389=ORIENTED_EDGE('',*,*,#3071,.F.);
#4390=ORIENTED_EDGE('',*,*,#3069,.F.);
#4391=ORIENTED_EDGE('',*,*,#3056,.F.);
#4392=ORIENTED_EDGE('',*,*,#3055,.F.);
#4393=ORIENTED_EDGE('',*,*,#3060,.F.);
#4394=ORIENTED_EDGE('',*,*,#3034,.F.);
#4395=ORIENTED_EDGE('',*,*,#3044,.F.);
#4396=ORIENTED_EDGE('',*,*,#3039,.F.);
#4397=ORIENTED_EDGE('',*,*,#3051,.F.);
#4398=ORIENTED_EDGE('',*,*,#3049,.F.);
#4399=ORIENTED_EDGE('',*,*,#2833,.F.);
#4400=ORIENTED_EDGE('',*,*,#2822,.F.);
#4401=ORIENTED_EDGE('',*,*,#2849,.F.);
#4402=ORIENTED_EDGE('',*,*,#2862,.F.);
#4403=ORIENTED_EDGE('',*,*,#3122,.T.);
#4404=ORIENTED_EDGE('',*,*,#3123,.T.);
#4405=ORIENTED_EDGE('',*,*,#3124,.T.);
#4406=ORIENTED_EDGE('',*,*,#3125,.T.);
#4407=ORIENTED_EDGE('',*,*,#3126,.T.);
#4408=ORIENTED_EDGE('',*,*,#3127,.T.);
#4409=ORIENTED_EDGE('',*,*,#3128,.T.);
#4410=ORIENTED_EDGE('',*,*,#3129,.T.);
#4411=ORIENTED_EDGE('',*,*,#3130,.T.);
#4412=ORIENTED_EDGE('',*,*,#3131,.T.);
#4413=ORIENTED_EDGE('',*,*,#3132,.T.);
#4414=ORIENTED_EDGE('',*,*,#3133,.T.);
#4415=ORIENTED_EDGE('',*,*,#3134,.T.);
#4416=ORIENTED_EDGE('',*,*,#3135,.T.);
#4417=ORIENTED_EDGE('',*,*,#3136,.T.);
#4418=ORIENTED_EDGE('',*,*,#3137,.F.);
#4419=ORIENTED_EDGE('',*,*,#3135,.F.);
#4420=ORIENTED_EDGE('',*,*,#3138,.F.);
#4421=ORIENTED_EDGE('',*,*,#3139,.F.);
#4422=ORIENTED_EDGE('',*,*,#3140,.T.);
#4423=ORIENTED_EDGE('',*,*,#3141,.T.);
#4424=ORIENTED_EDGE('',*,*,#3127,.F.);
#4425=ORIENTED_EDGE('',*,*,#3142,.F.);
#4426=ORIENTED_EDGE('',*,*,#3143,.F.);
#4427=ORIENTED_EDGE('',*,*,#3144,.T.);
#4428=ORIENTED_EDGE('',*,*,#3125,.F.);
#4429=ORIENTED_EDGE('',*,*,#3145,.F.);
#4430=ORIENTED_EDGE('',*,*,#3146,.F.);
#4431=ORIENTED_EDGE('',*,*,#3147,.F.);
#4432=ORIENTED_EDGE('',*,*,#3148,.F.);
#4433=ORIENTED_EDGE('',*,*,#3149,.T.);
#4434=ORIENTED_EDGE('',*,*,#3123,.F.);
#4435=ORIENTED_EDGE('',*,*,#3150,.F.);
#4436=ORIENTED_EDGE('',*,*,#3151,.T.);
#4437=ORIENTED_EDGE('',*,*,#3152,.T.);
#4438=ORIENTED_EDGE('',*,*,#3151,.F.);
#4439=ORIENTED_EDGE('',*,*,#3153,.F.);
#4440=ORIENTED_EDGE('',*,*,#3154,.T.);
#4441=ORIENTED_EDGE('',*,*,#3155,.T.);
#4442=ORIENTED_EDGE('',*,*,#3129,.F.);
#4443=ORIENTED_EDGE('',*,*,#3156,.F.);
#4444=ORIENTED_EDGE('',*,*,#3157,.T.);
#4445=ORIENTED_EDGE('',*,*,#3158,.T.);
#4446=ORIENTED_EDGE('',*,*,#3157,.F.);
#4447=ORIENTED_EDGE('',*,*,#3159,.F.);
#4448=ORIENTED_EDGE('',*,*,#3160,.F.);
#4449=ORIENTED_EDGE('',*,*,#3161,.F.);
#4450=ORIENTED_EDGE('',*,*,#3154,.F.);
#4451=ORIENTED_EDGE('',*,*,#3162,.F.);
#4452=ORIENTED_EDGE('',*,*,#3140,.F.);
#4453=ORIENTED_EDGE('',*,*,#3163,.F.);
#4454=ORIENTED_EDGE('',*,*,#3143,.T.);
#4455=ORIENTED_EDGE('',*,*,#3164,.F.);
#4456=ORIENTED_EDGE('',*,*,#3148,.T.);
#4457=ORIENTED_EDGE('',*,*,#3165,.F.);
#4458=ORIENTED_EDGE('',*,*,#3136,.F.);
#4459=ORIENTED_EDGE('',*,*,#3166,.F.);
#4460=ORIENTED_EDGE('',*,*,#3167,.F.);
#4461=ORIENTED_EDGE('',*,*,#3152,.F.);
#4462=ORIENTED_EDGE('',*,*,#3158,.F.);
#4463=ORIENTED_EDGE('',*,*,#3156,.T.);
#4464=ORIENTED_EDGE('',*,*,#3150,.T.);
#4465=ORIENTED_EDGE('',*,*,#3141,.F.);
#4466=ORIENTED_EDGE('',*,*,#3162,.T.);
#4467=ORIENTED_EDGE('',*,*,#3153,.T.);
#4468=ORIENTED_EDGE('',*,*,#3128,.F.);
#4469=ORIENTED_EDGE('',*,*,#3144,.F.);
#4470=ORIENTED_EDGE('',*,*,#3163,.T.);
#4471=ORIENTED_EDGE('',*,*,#3139,.T.);
#4472=ORIENTED_EDGE('',*,*,#3126,.F.);
#4473=ORIENTED_EDGE('',*,*,#3149,.F.);
#4474=ORIENTED_EDGE('',*,*,#3164,.T.);
#4475=ORIENTED_EDGE('',*,*,#3142,.T.);
#4476=ORIENTED_EDGE('',*,*,#3124,.F.);
#4477=ORIENTED_EDGE('',*,*,#3137,.T.);
#4478=ORIENTED_EDGE('',*,*,#3165,.T.);
#4479=ORIENTED_EDGE('',*,*,#3147,.T.);
#4480=ORIENTED_EDGE('',*,*,#3122,.F.);
#4481=ORIENTED_EDGE('',*,*,#3168,.F.);
#4482=ORIENTED_EDGE('',*,*,#3169,.T.);
#4483=ORIENTED_EDGE('',*,*,#3170,.F.);
#4484=ORIENTED_EDGE('',*,*,#3159,.T.);
#4485=ORIENTED_EDGE('',*,*,#3171,.F.);
#4486=ORIENTED_EDGE('',*,*,#3172,.T.);
#4487=ORIENTED_EDGE('',*,*,#3173,.T.);
#4488=ORIENTED_EDGE('',*,*,#3174,.T.);
#4489=ORIENTED_EDGE('',*,*,#3132,.F.);
#4490=ORIENTED_EDGE('',*,*,#3146,.T.);
#4491=ORIENTED_EDGE('',*,*,#3175,.T.);
#4492=ORIENTED_EDGE('',*,*,#3176,.F.);
#4493=ORIENTED_EDGE('',*,*,#3169,.F.);
#4494=ORIENTED_EDGE('',*,*,#3177,.F.);
#4495=ORIENTED_EDGE('',*,*,#3175,.F.);
#4496=ORIENTED_EDGE('',*,*,#3145,.T.);
#4497=ORIENTED_EDGE('',*,*,#3178,.T.);
#4498=ORIENTED_EDGE('',*,*,#3172,.F.);
#4499=ORIENTED_EDGE('',*,*,#3179,.F.);
#4500=ORIENTED_EDGE('',*,*,#3173,.F.);
#4501=ORIENTED_EDGE('',*,*,#3178,.F.);
#4502=ORIENTED_EDGE('',*,*,#3174,.F.);
#4503=ORIENTED_EDGE('',*,*,#3179,.T.);
#4504=ORIENTED_EDGE('',*,*,#3171,.T.);
#4505=ORIENTED_EDGE('',*,*,#3167,.T.);
#4506=ORIENTED_EDGE('',*,*,#3180,.T.);
#4507=ORIENTED_EDGE('',*,*,#3133,.F.);
#4508=ORIENTED_EDGE('',*,*,#3180,.F.);
#4509=ORIENTED_EDGE('',*,*,#3166,.T.);
#4510=ORIENTED_EDGE('',*,*,#3138,.T.);
#4511=ORIENTED_EDGE('',*,*,#3134,.F.);
#4512=ORIENTED_EDGE('',*,*,#3181,.F.);
#4513=ORIENTED_EDGE('',*,*,#3160,.T.);
#4514=ORIENTED_EDGE('',*,*,#3170,.T.);
#4515=ORIENTED_EDGE('',*,*,#3176,.T.);
#4516=ORIENTED_EDGE('',*,*,#3177,.T.);
#4517=ORIENTED_EDGE('',*,*,#3168,.T.);
#4518=ORIENTED_EDGE('',*,*,#3131,.F.);
#4519=ORIENTED_EDGE('',*,*,#3155,.F.);
#4520=ORIENTED_EDGE('',*,*,#3161,.T.);
#4521=ORIENTED_EDGE('',*,*,#3181,.T.);
#4522=ORIENTED_EDGE('',*,*,#3130,.F.);
#4523=ORIENTED_EDGE('',*,*,#3182,.T.);
#4524=ORIENTED_EDGE('',*,*,#3183,.T.);
#4525=ORIENTED_EDGE('',*,*,#3184,.T.);
#4526=ORIENTED_EDGE('',*,*,#3185,.T.);
#4527=ORIENTED_EDGE('',*,*,#3183,.F.);
#4528=ORIENTED_EDGE('',*,*,#3186,.T.);
#4529=ORIENTED_EDGE('',*,*,#3187,.T.);
#4530=ORIENTED_EDGE('',*,*,#3188,.T.);
#4531=ORIENTED_EDGE('',*,*,#3182,.F.);
#4532=ORIENTED_EDGE('',*,*,#3189,.T.);
#4533=ORIENTED_EDGE('',*,*,#3188,.F.);
#4534=ORIENTED_EDGE('',*,*,#3189,.F.);
#4535=ORIENTED_EDGE('',*,*,#3186,.F.);
#4536=ORIENTED_EDGE('',*,*,#3187,.F.);
#4537=ORIENTED_EDGE('',*,*,#3190,.T.);
#4538=ORIENTED_EDGE('',*,*,#3184,.F.);
#4539=ORIENTED_EDGE('',*,*,#3185,.F.);
#4540=ORIENTED_EDGE('',*,*,#3190,.F.);
#4541=ORIENTED_EDGE('',*,*,#3191,.F.);
#4542=ORIENTED_EDGE('',*,*,#3192,.T.);
#4543=ORIENTED_EDGE('',*,*,#3193,.F.);
#4544=ORIENTED_EDGE('',*,*,#3194,.T.);
#4545=ORIENTED_EDGE('',*,*,#3191,.T.);
#4546=ORIENTED_EDGE('',*,*,#3194,.F.);
#4547=ORIENTED_EDGE('',*,*,#3193,.T.);
#4548=ORIENTED_EDGE('',*,*,#3195,.F.);
#4549=ORIENTED_EDGE('',*,*,#3192,.F.);
#4550=ORIENTED_EDGE('',*,*,#3196,.T.);
#4551=ORIENTED_EDGE('',*,*,#3195,.T.);
#4552=ORIENTED_EDGE('',*,*,#3196,.F.);
#4553=ORIENTED_EDGE('',*,*,#3197,.T.);
#4554=ORIENTED_EDGE('',*,*,#3198,.T.);
#4555=ORIENTED_EDGE('',*,*,#3199,.T.);
#4556=ORIENTED_EDGE('',*,*,#3198,.F.);
#4557=ORIENTED_EDGE('',*,*,#3200,.T.);
#4558=ORIENTED_EDGE('',*,*,#3201,.F.);
#4559=ORIENTED_EDGE('',*,*,#3199,.F.);
#4560=ORIENTED_EDGE('',*,*,#3197,.F.);
#4561=ORIENTED_EDGE('',*,*,#3202,.T.);
#4562=ORIENTED_EDGE('',*,*,#3203,.T.);
#4563=ORIENTED_EDGE('',*,*,#3202,.F.);
#4564=ORIENTED_EDGE('',*,*,#3200,.F.);
#4565=ORIENTED_EDGE('',*,*,#3204,.T.);
#4566=ORIENTED_EDGE('',*,*,#3205,.T.);
#4567=ORIENTED_EDGE('',*,*,#3201,.T.);
#4568=ORIENTED_EDGE('',*,*,#3205,.F.);
#4569=ORIENTED_EDGE('',*,*,#3206,.T.);
#4570=ORIENTED_EDGE('',*,*,#3207,.F.);
#4571=ORIENTED_EDGE('',*,*,#3208,.T.);
#4572=ORIENTED_EDGE('',*,*,#3206,.F.);
#4573=ORIENTED_EDGE('',*,*,#3204,.F.);
#4574=ORIENTED_EDGE('',*,*,#3208,.F.);
#4575=ORIENTED_EDGE('',*,*,#3209,.T.);
#4576=ORIENTED_EDGE('',*,*,#3210,.T.);
#4577=ORIENTED_EDGE('',*,*,#3211,.T.);
#4578=ORIENTED_EDGE('',*,*,#3210,.F.);
#4579=ORIENTED_EDGE('',*,*,#3212,.T.);
#4580=ORIENTED_EDGE('',*,*,#3213,.F.);
#4581=ORIENTED_EDGE('',*,*,#3211,.F.);
#4582=ORIENTED_EDGE('',*,*,#3214,.F.);
#4583=ORIENTED_EDGE('',*,*,#3215,.T.);
#4584=ORIENTED_EDGE('',*,*,#3212,.F.);
#4585=ORIENTED_EDGE('',*,*,#3209,.F.);
#4586=ORIENTED_EDGE('',*,*,#3215,.F.);
#4587=ORIENTED_EDGE('',*,*,#3216,.T.);
#4588=ORIENTED_EDGE('',*,*,#3217,.T.);
#4589=ORIENTED_EDGE('',*,*,#3213,.T.);
#4590=ORIENTED_EDGE('',*,*,#3217,.F.);
#4591=ORIENTED_EDGE('',*,*,#3218,.T.);
#4592=ORIENTED_EDGE('',*,*,#3216,.F.);
#4593=ORIENTED_EDGE('',*,*,#3219,.T.);
#4594=ORIENTED_EDGE('',*,*,#3220,.T.);
#4595=ORIENTED_EDGE('',*,*,#3219,.F.);
#4596=ORIENTED_EDGE('',*,*,#3218,.F.);
#4597=ORIENTED_EDGE('',*,*,#3221,.F.);
#4598=ORIENTED_EDGE('',*,*,#3214,.T.);
#4599=ORIENTED_EDGE('',*,*,#3222,.F.);
#4600=ORIENTED_EDGE('',*,*,#3223,.T.);
#4601=ORIENTED_EDGE('',*,*,#3221,.T.);
#4602=ORIENTED_EDGE('',*,*,#3223,.F.);
#4603=ORIENTED_EDGE('',*,*,#3222,.T.);
#4604=ORIENTED_EDGE('',*,*,#3224,.F.);
#4605=ORIENTED_EDGE('',*,*,#3225,.F.);
#4606=ORIENTED_EDGE('',*,*,#3226,.T.);
#4607=ORIENTED_EDGE('',*,*,#3224,.T.);
#4608=ORIENTED_EDGE('',*,*,#3226,.F.);
#4609=ORIENTED_EDGE('',*,*,#3227,.F.);
#4610=ORIENTED_EDGE('',*,*,#3228,.T.);
#4611=ORIENTED_EDGE('',*,*,#3225,.T.);
#4612=ORIENTED_EDGE('',*,*,#3228,.F.);
#4613=ORIENTED_EDGE('',*,*,#3229,.F.);
#4614=ORIENTED_EDGE('',*,*,#3230,.T.);
#4615=ORIENTED_EDGE('',*,*,#3227,.T.);
#4616=ORIENTED_EDGE('',*,*,#3230,.F.);
#4617=ORIENTED_EDGE('',*,*,#3229,.T.);
#4618=ORIENTED_EDGE('',*,*,#3231,.T.);
#4619=ORIENTED_EDGE('',*,*,#3232,.F.);
#4620=ORIENTED_EDGE('',*,*,#3231,.F.);
#4621=ORIENTED_EDGE('',*,*,#3233,.F.);
#4622=ORIENTED_EDGE('',*,*,#3234,.T.);
#4623=ORIENTED_EDGE('',*,*,#3232,.T.);
#4624=ORIENTED_EDGE('',*,*,#3234,.F.);
#4625=ORIENTED_EDGE('',*,*,#3235,.F.);
#4626=ORIENTED_EDGE('',*,*,#3233,.T.);
#4627=ORIENTED_EDGE('',*,*,#3236,.F.);
#4628=ORIENTED_EDGE('',*,*,#3237,.T.);
#4629=ORIENTED_EDGE('',*,*,#3235,.T.);
#4630=ORIENTED_EDGE('',*,*,#3237,.F.);
#4631=ORIENTED_EDGE('',*,*,#3236,.T.);
#4632=ORIENTED_EDGE('',*,*,#3203,.F.);
#4633=ORIENTED_EDGE('',*,*,#3207,.T.);
#4634=ORIENTED_EDGE('',*,*,#3238,.F.);
#4635=ORIENTED_EDGE('',*,*,#3239,.F.);
#4636=ORIENTED_EDGE('',*,*,#3240,.T.);
#4637=ORIENTED_EDGE('',*,*,#3238,.T.);
#4638=ORIENTED_EDGE('',*,*,#3240,.F.);
#4639=ORIENTED_EDGE('',*,*,#3241,.F.);
#4640=ORIENTED_EDGE('',*,*,#3239,.T.);
#4641=ORIENTED_EDGE('',*,*,#3242,.F.);
#4642=ORIENTED_EDGE('',*,*,#3243,.T.);
#4643=ORIENTED_EDGE('',*,*,#3241,.T.);
#4644=ORIENTED_EDGE('',*,*,#3243,.F.);
#4645=ORIENTED_EDGE('',*,*,#3242,.T.);
#4646=ORIENTED_EDGE('',*,*,#3244,.F.);
#4647=ORIENTED_EDGE('',*,*,#3245,.F.);
#4648=ORIENTED_EDGE('',*,*,#3246,.T.);
#4649=ORIENTED_EDGE('',*,*,#3244,.T.);
#4650=ORIENTED_EDGE('',*,*,#3246,.F.);
#4651=ORIENTED_EDGE('',*,*,#3220,.F.);
#4652=ORIENTED_EDGE('',*,*,#3245,.T.);
#4653=ORIENTED_EDGE('',*,*,#3247,.F.);
#4654=ORIENTED_EDGE('',*,*,#3248,.T.);
#4655=ORIENTED_EDGE('',*,*,#3249,.F.);
#4656=ORIENTED_EDGE('',*,*,#3250,.T.);
#4657=ORIENTED_EDGE('',*,*,#3247,.T.);
#4658=ORIENTED_EDGE('',*,*,#3250,.F.);
#4659=ORIENTED_EDGE('',*,*,#3249,.T.);
#4660=ORIENTED_EDGE('',*,*,#3251,.F.);
#4661=ORIENTED_EDGE('',*,*,#3252,.F.);
#4662=ORIENTED_EDGE('',*,*,#3253,.T.);
#4663=ORIENTED_EDGE('',*,*,#3251,.T.);
#4664=ORIENTED_EDGE('',*,*,#3253,.F.);
#4665=ORIENTED_EDGE('',*,*,#3254,.F.);
#4666=ORIENTED_EDGE('',*,*,#3255,.T.);
#4667=ORIENTED_EDGE('',*,*,#3252,.T.);
#4668=ORIENTED_EDGE('',*,*,#3255,.F.);
#4669=ORIENTED_EDGE('',*,*,#3256,.F.);
#4670=ORIENTED_EDGE('',*,*,#3254,.T.);
#4671=ORIENTED_EDGE('',*,*,#3248,.F.);
#4672=ORIENTED_EDGE('',*,*,#3257,.T.);
#4673=ORIENTED_EDGE('',*,*,#3256,.T.);
#4674=ORIENTED_EDGE('',*,*,#3257,.F.);
#4675=ORIENTED_EDGE('',*,*,#3258,.T.);
#4676=ORIENTED_EDGE('',*,*,#3259,.F.);
#4677=ORIENTED_EDGE('',*,*,#3258,.F.);
#4678=ORIENTED_EDGE('',*,*,#3260,.T.);
#4679=ORIENTED_EDGE('',*,*,#3261,.T.);
#4680=ORIENTED_EDGE('',*,*,#3260,.F.);
#4681=ORIENTED_EDGE('',*,*,#3261,.F.);
#4682=ORIENTED_EDGE('',*,*,#3262,.T.);
#4683=ORIENTED_EDGE('',*,*,#3262,.F.);
#4684=ORIENTED_EDGE('',*,*,#3263,.T.);
#4685=ORIENTED_EDGE('',*,*,#3259,.T.);
#4686=ORIENTED_EDGE('',*,*,#3263,.F.);
#4687=ORIENTED_EDGE('',*,*,#3264,.T.);
#4688=ORIENTED_EDGE('',*,*,#3265,.F.);
#4689=ORIENTED_EDGE('',*,*,#3264,.F.);
#4690=ORIENTED_EDGE('',*,*,#3266,.T.);
#4691=ORIENTED_EDGE('',*,*,#3267,.T.);
#4692=ORIENTED_EDGE('',*,*,#3266,.F.);
#4693=ORIENTED_EDGE('',*,*,#3267,.F.);
#4694=ORIENTED_EDGE('',*,*,#3268,.T.);
#4695=ORIENTED_EDGE('',*,*,#3269,.T.);
#4696=ORIENTED_EDGE('',*,*,#3270,.T.);
#4697=ORIENTED_EDGE('',*,*,#3268,.F.);
#4698=ORIENTED_EDGE('',*,*,#3270,.F.);
#4699=ORIENTED_EDGE('',*,*,#3269,.F.);
#4700=ORIENTED_EDGE('',*,*,#3271,.T.);
#4701=ORIENTED_EDGE('',*,*,#3272,.T.);
#4702=ORIENTED_EDGE('',*,*,#3271,.F.);
#4703=ORIENTED_EDGE('',*,*,#3273,.T.);
#4704=ORIENTED_EDGE('',*,*,#3272,.F.);
#4705=ORIENTED_EDGE('',*,*,#3265,.T.);
#4706=ORIENTED_EDGE('',*,*,#3274,.T.);
#4707=ORIENTED_EDGE('',*,*,#3273,.F.);
#4708=ORIENTED_EDGE('',*,*,#3274,.F.);
#4709=PLANE('',#5261);
#4710=PLANE('',#5270);
#4711=PLANE('',#5271);
#4712=PLANE('',#5272);
#4713=PLANE('',#5275);
#4714=PLANE('',#5279);
#4715=PLANE('',#5283);
#4716=PLANE('',#5292);
#4717=PLANE('',#5293);
#4718=PLANE('',#5298);
#4719=PLANE('',#5309);
#4720=PLANE('',#5310);
#4721=PLANE('',#5311);
#4722=PLANE('',#5312);
#4723=PLANE('',#5313);
#4724=PLANE('',#5314);
#4725=PLANE('',#5315);
#4726=PLANE('',#5316);
#4727=PLANE('',#5317);
#4728=PLANE('',#5318);
#4729=PLANE('',#5319);
#4730=PLANE('',#5321);
#4731=PLANE('',#5323);
#4732=PLANE('',#5325);
#4733=PLANE('',#5327);
#4734=PLANE('',#5329);
#4735=PLANE('',#5331);
#4736=PLANE('',#5332);
#4737=PLANE('',#5334);
#4738=PLANE('',#5336);
#4739=PLANE('',#5338);
#4740=PLANE('',#5339);
#4741=PLANE('',#5340);
#4742=PLANE('',#5341);
#4743=PLANE('',#5343);
#4744=PLANE('',#5345);
#4745=PLANE('',#5347);
#4746=PLANE('',#5348);
#4747=PLANE('',#5349);
#4748=PLANE('',#5350);
#4749=PLANE('',#5352);
#4750=PLANE('',#5354);
#4751=PLANE('',#5355);
#4752=PLANE('',#5356);
#4753=PLANE('',#5357);
#4754=PLANE('',#5358);
#4755=PLANE('',#5359);
#4756=PLANE('',#5360);
#4757=PLANE('',#5361);
#4758=PLANE('',#5365);
#4759=PLANE('',#5371);
#4760=PLANE('',#5375);
#4761=PLANE('',#5381);
#4762=PLANE('',#5382);
#4763=PLANE('',#5383);
#4764=PLANE('',#5389);
#4765=PLANE('',#5390);
#4766=PLANE('',#5392);
#4767=PLANE('',#5394);
#4768=PLANE('',#5396);
#4769=PLANE('',#5398);
#4770=PLANE('',#5400);
#4771=PLANE('',#5402);
#4772=PLANE('',#5403);
#4773=PLANE('',#5405);
#4774=PLANE('',#5407);
#4775=PLANE('',#5409);
#4776=PLANE('',#5411);
#4777=PLANE('',#5413);
#4778=PLANE('',#5431);
#4779=PLANE('',#5434);
#4780=PLANE('',#5435);
#4781=PLANE('',#5438);
#4782=PLANE('',#5439);
#4783=PLANE('',#5442);
#4784=PLANE('',#5445);
#4785=PLANE('',#5448);
#4786=PLANE('',#5449);
#4787=PLANE('',#5452);
#4788=PLANE('',#5455);
#4789=PLANE('',#5456);
#4790=PLANE('',#5459);
#4791=PLANE('',#5462);
#4792=PLANE('',#5463);
#4793=PLANE('',#5466);
#4794=PLANE('',#5469);
#4795=PLANE('',#5470);
#4796=PLANE('',#5473);
#4797=PLANE('',#5474);
#4798=PLANE('',#5477);
#4799=PLANE('',#5480);
#4800=PLANE('',#5481);
#4801=PLANE('',#5484);
#4802=PLANE('',#5503);
#4803=PLANE('',#5505);
#4804=PLANE('',#5506);
#4805=PLANE('',#5508);
#4806=PLANE('',#5509);
#4807=PLANE('',#5511);
#4808=PLANE('',#5513);
#4809=PLANE('',#5515);
#4810=PLANE('',#5516);
#4811=PLANE('',#5518);
#4812=PLANE('',#5519);
#4813=PLANE('',#5521);
#4814=PLANE('',#5522);
#4815=PLANE('',#5523);
#4816=PLANE('',#5524);
#4817=PLANE('',#5542);
#4818=PLANE('',#5543);
#4819=PLANE('',#5546);
#4820=PLANE('',#5547);
#4821=PLANE('',#5550);
#4822=PLANE('',#5551);
#4823=PLANE('',#5554);
#4824=PLANE('',#5555);
#4825=PLANE('',#5558);
#4826=PLANE('',#5559);
#4827=PLANE('',#5562);
#4828=PLANE('',#5563);
#4829=PLANE('',#5566);
#4830=PLANE('',#5567);
#4831=PLANE('',#5570);
#4832=PLANE('',#5571);
#4833=PLANE('',#5574);
#4834=PLANE('',#5575);
#4835=PLANE('',#5578);
#4836=PLANE('',#5579);
#4837=PLANE('',#5582);
#4838=PLANE('',#5583);
#4839=PLANE('',#5586);
#4840=PLANE('',#5587);
#4841=PLANE('',#5590);
#4842=PLANE('',#5591);
#4843=PLANE('',#5594);
#4844=PLANE('',#5595);
#4845=PLANE('',#5598);
#4846=PLANE('',#5599);
#4847=PLANE('',#5602);
#4848=PLANE('',#5603);
#4849=PLANE('',#5624);
#4850=PLANE('',#5633);
#4851=PLANE('',#5634);
#4852=PLANE('',#5635);
#4853=PLANE('',#5638);
#4854=PLANE('',#5642);
#4855=PLANE('',#5646);
#4856=PLANE('',#5655);
#4857=PLANE('',#5656);
#4858=PLANE('',#5661);
#4859=PLANE('',#5677);
#4860=PLANE('',#5679);
#4861=PLANE('',#5687);
#4862=PLANE('',#5692);
#4863=PLANE('',#5700);
#4864=PLANE('',#5713);
#4865=PLANE('',#5722);
#4866=PLANE('',#5726);
#4867=PLANE('',#5738);
#4868=PLANE('',#5742);
#4869=PLANE('',#5743);
#4870=PLANE('',#5747);
#4871=PLANE('',#5751);
#4872=PLANE('',#5755);
#4873=PLANE('',#5757);
#4874=PLANE('',#5762);
#4875=PLANE('',#5768);
#4876=PLANE('',#5772);
#4877=PLANE('',#5777);
#4878=PLANE('',#5781);
#4879=PLANE('',#5786);
#4880=PLANE('',#5792);
#4881=ADVANCED_FACE('',(#308),#4709,.T.);
#4882=ADVANCED_FACE('',(#309),#4710,.T.);
#4883=ADVANCED_FACE('',(#310),#4711,.T.);
#4884=ADVANCED_FACE('',(#311,#238,#239),#4712,.F.);
#4885=ADVANCED_FACE('',(#312),#4713,.F.);
#4886=ADVANCED_FACE('',(#313),#153,.F.);
#4887=ADVANCED_FACE('',(#314),#4714,.T.);
#4888=ADVANCED_FACE('',(#315),#154,.F.);
#4889=ADVANCED_FACE('',(#316,#240,#241),#4715,.F.);
#4890=ADVANCED_FACE('',(#317),#4716,.F.);
#4891=ADVANCED_FACE('',(#318),#4717,.F.);
#4892=ADVANCED_FACE('',(#319),#155,.T.);
#4893=ADVANCED_FACE('',(#320),#156,.T.);
#4894=ADVANCED_FACE('',(#321),#157,.T.);
#4895=ADVANCED_FACE('',(#322),#158,.T.);
#4896=ADVANCED_FACE('',(#323),#4718,.T.);
#4897=ADVANCED_FACE('',(#324),#159,.F.);
#4898=ADVANCED_FACE('',(#325),#160,.F.);
#4899=ADVANCED_FACE('',(#326),#161,.T.);
#4900=ADVANCED_FACE('',(#327),#162,.F.);
#4901=ADVANCED_FACE('',(#328),#163,.T.);
#4902=ADVANCED_FACE('',(#329),#164,.F.);
#4903=ADVANCED_FACE('',(#330),#4719,.F.);
#4904=ADVANCED_FACE('',(#331),#4720,.F.);
#4905=ADVANCED_FACE('',(#332),#4721,.F.);
#4906=ADVANCED_FACE('',(#333),#4722,.T.);
#4907=ADVANCED_FACE('',(#334),#4723,.T.);
#4908=ADVANCED_FACE('',(#335),#4724,.T.);
#4909=ADVANCED_FACE('',(#336),#4725,.T.);
#4910=ADVANCED_FACE('',(#337),#4726,.T.);
#4911=ADVANCED_FACE('',(#338),#4727,.T.);
#4912=ADVANCED_FACE('',(#339,#242,#243,#244,#245,#246,#247,#248,#249),#4728,
 .F.);
#4913=ADVANCED_FACE('',(#340),#4729,.T.);
#4914=ADVANCED_FACE('',(#341),#4730,.F.);
#4915=ADVANCED_FACE('',(#342),#4731,.T.);
#4916=ADVANCED_FACE('',(#343),#4732,.F.);
#4917=ADVANCED_FACE('',(#344),#4733,.T.);
#4918=ADVANCED_FACE('',(#345),#4734,.T.);
#4919=ADVANCED_FACE('',(#346),#4735,.F.);
#4920=ADVANCED_FACE('',(#347),#4736,.F.);
#4921=ADVANCED_FACE('',(#348),#4737,.T.);
#4922=ADVANCED_FACE('',(#349),#4738,.F.);
#4923=ADVANCED_FACE('',(#350),#4739,.T.);
#4924=ADVANCED_FACE('',(#351),#4740,.T.);
#4925=ADVANCED_FACE('',(#352,#250,#251,#252,#253,#254,#255,#256,#257),#4741,
 .T.);
#4926=ADVANCED_FACE('',(#353),#4742,.T.);
#4927=ADVANCED_FACE('',(#354),#4743,.F.);
#4928=ADVANCED_FACE('',(#355),#4744,.F.);
#4929=ADVANCED_FACE('',(#356),#4745,.F.);
#4930=ADVANCED_FACE('',(#357),#4746,.F.);
#4931=ADVANCED_FACE('',(#358),#4747,.F.);
#4932=ADVANCED_FACE('',(#359),#4748,.T.);
#4933=ADVANCED_FACE('',(#360),#4749,.F.);
#4934=ADVANCED_FACE('',(#361),#4750,.F.);
#4935=ADVANCED_FACE('',(#362),#4751,.T.);
#4936=ADVANCED_FACE('',(#363),#4752,.T.);
#4937=ADVANCED_FACE('',(#364),#4753,.T.);
#4938=ADVANCED_FACE('',(#365),#4754,.T.);
#4939=ADVANCED_FACE('',(#366),#4755,.F.);
#4940=ADVANCED_FACE('',(#367),#4756,.T.);
#4941=ADVANCED_FACE('',(#368),#4757,.F.);
#4942=ADVANCED_FACE('',(#369,#258,#259,#260,#261,#262),#4758,.F.);
#4943=ADVANCED_FACE('',(#370),#4759,.T.);
#4944=ADVANCED_FACE('',(#371,#263,#264,#265,#266,#267),#4760,.T.);
#4945=ADVANCED_FACE('',(#372),#4761,.T.);
#4946=ADVANCED_FACE('',(#373),#4762,.F.);
#4947=ADVANCED_FACE('',(#374),#4763,.F.);
#4948=ADVANCED_FACE('',(#375),#165,.F.);
#4949=ADVANCED_FACE('',(#376),#166,.F.);
#4950=ADVANCED_FACE('',(#377),#167,.F.);
#4951=ADVANCED_FACE('',(#378),#168,.F.);
#4952=ADVANCED_FACE('',(#379),#169,.F.);
#4953=ADVANCED_FACE('',(#380),#4764,.F.);
#4954=ADVANCED_FACE('',(#381),#4765,.T.);
#4955=ADVANCED_FACE('',(#382),#4766,.T.);
#4956=ADVANCED_FACE('',(#383),#4767,.F.);
#4957=ADVANCED_FACE('',(#384),#4768,.T.);
#4958=ADVANCED_FACE('',(#385),#4769,.F.);
#4959=ADVANCED_FACE('',(#386),#4770,.T.);
#4960=ADVANCED_FACE('',(#387),#4771,.F.);
#4961=ADVANCED_FACE('',(#388),#4772,.F.);
#4962=ADVANCED_FACE('',(#389),#4773,.T.);
#4963=ADVANCED_FACE('',(#390),#4774,.F.);
#4964=ADVANCED_FACE('',(#391),#4775,.T.);
#4965=ADVANCED_FACE('',(#392),#4776,.F.);
#4966=ADVANCED_FACE('',(#393),#4777,.T.);
#4967=ADVANCED_FACE('',(#394,#268,#269,#270,#271,#272,#273,#274,#275),#170,
 .F.);
#4968=ADVANCED_FACE('',(#395),#4778,.F.);
#4969=ADVANCED_FACE('',(#396),#4779,.F.);
#4970=ADVANCED_FACE('',(#397),#4780,.T.);
#4971=ADVANCED_FACE('',(#398),#4781,.T.);
#4972=ADVANCED_FACE('',(#399),#4782,.F.);
#4973=ADVANCED_FACE('',(#400),#4783,.T.);
#4974=ADVANCED_FACE('',(#401),#4784,.F.);
#4975=ADVANCED_FACE('',(#402),#4785,.F.);
#4976=ADVANCED_FACE('',(#403),#4786,.T.);
#4977=ADVANCED_FACE('',(#404),#4787,.F.);
#4978=ADVANCED_FACE('',(#405),#4788,.F.);
#4979=ADVANCED_FACE('',(#406),#4789,.T.);
#4980=ADVANCED_FACE('',(#407),#4790,.F.);
#4981=ADVANCED_FACE('',(#408),#4791,.F.);
#4982=ADVANCED_FACE('',(#409),#4792,.T.);
#4983=ADVANCED_FACE('',(#410),#4793,.F.);
#4984=ADVANCED_FACE('',(#411),#4794,.F.);
#4985=ADVANCED_FACE('',(#412),#4795,.T.);
#4986=ADVANCED_FACE('',(#413),#4796,.T.);
#4987=ADVANCED_FACE('',(#414),#4797,.F.);
#4988=ADVANCED_FACE('',(#415),#4798,.T.);
#4989=ADVANCED_FACE('',(#416),#4799,.T.);
#4990=ADVANCED_FACE('',(#417),#4800,.F.);
#4991=ADVANCED_FACE('',(#418),#4801,.T.);
#4992=ADVANCED_FACE('',(#419),#171,.T.);
#4993=ADVANCED_FACE('',(#420),#172,.T.);
#4994=ADVANCED_FACE('',(#421),#173,.T.);
#4995=ADVANCED_FACE('',(#422),#174,.T.);
#4996=ADVANCED_FACE('',(#423),#175,.T.);
#4997=ADVANCED_FACE('',(#424),#176,.T.);
#4998=ADVANCED_FACE('',(#425),#177,.T.);
#4999=ADVANCED_FACE('',(#426),#178,.T.);
#5000=ADVANCED_FACE('',(#427),#179,.T.);
#5001=ADVANCED_FACE('',(#428),#180,.T.);
#5002=ADVANCED_FACE('',(#429),#181,.T.);
#5003=ADVANCED_FACE('',(#430),#182,.T.);
#5004=ADVANCED_FACE('',(#431),#183,.T.);
#5005=ADVANCED_FACE('',(#432),#184,.T.);
#5006=ADVANCED_FACE('',(#433),#185,.T.);
#5007=ADVANCED_FACE('',(#434),#186,.T.);
#5008=ADVANCED_FACE('',(#435),#4802,.T.);
#5009=ADVANCED_FACE('',(#436),#4803,.F.);
#5010=ADVANCED_FACE('',(#437),#4804,.F.);
#5011=ADVANCED_FACE('',(#438),#4805,.F.);
#5012=ADVANCED_FACE('',(#439),#4806,.F.);
#5013=ADVANCED_FACE('',(#440),#4807,.F.);
#5014=ADVANCED_FACE('',(#441),#4808,.T.);
#5015=ADVANCED_FACE('',(#442),#4809,.F.);
#5016=ADVANCED_FACE('',(#443),#4810,.T.);
#5017=ADVANCED_FACE('',(#444),#4811,.F.);
#5018=ADVANCED_FACE('',(#445),#4812,.F.);
#5019=ADVANCED_FACE('',(#446),#4813,.T.);
#5020=ADVANCED_FACE('',(#447),#4814,.T.);
#5021=ADVANCED_FACE('',(#448),#4815,.T.);
#5022=ADVANCED_FACE('',(#449),#4816,.T.);
#5023=ADVANCED_FACE('',(#450,#276,#277,#278,#279,#280,#281,#282,#283),#187,
 .F.);
#5024=ADVANCED_FACE('',(#451),#4817,.T.);
#5025=ADVANCED_FACE('',(#452),#4818,.F.);
#5026=ADVANCED_FACE('',(#453),#4819,.F.);
#5027=ADVANCED_FACE('',(#454),#4820,.T.);
#5028=ADVANCED_FACE('',(#455),#4821,.T.);
#5029=ADVANCED_FACE('',(#456),#4822,.F.);
#5030=ADVANCED_FACE('',(#457),#4823,.F.);
#5031=ADVANCED_FACE('',(#458),#4824,.T.);
#5032=ADVANCED_FACE('',(#459),#4825,.T.);
#5033=ADVANCED_FACE('',(#460),#4826,.F.);
#5034=ADVANCED_FACE('',(#461),#4827,.F.);
#5035=ADVANCED_FACE('',(#462),#4828,.T.);
#5036=ADVANCED_FACE('',(#463),#4829,.T.);
#5037=ADVANCED_FACE('',(#464),#4830,.F.);
#5038=ADVANCED_FACE('',(#465),#4831,.F.);
#5039=ADVANCED_FACE('',(#466),#4832,.T.);
#5040=ADVANCED_FACE('',(#467),#4833,.T.);
#5041=ADVANCED_FACE('',(#468),#4834,.F.);
#5042=ADVANCED_FACE('',(#469),#4835,.F.);
#5043=ADVANCED_FACE('',(#470),#4836,.T.);
#5044=ADVANCED_FACE('',(#471),#4837,.T.);
#5045=ADVANCED_FACE('',(#472),#4838,.F.);
#5046=ADVANCED_FACE('',(#473),#4839,.F.);
#5047=ADVANCED_FACE('',(#474),#4840,.T.);
#5048=ADVANCED_FACE('',(#475),#4841,.T.);
#5049=ADVANCED_FACE('',(#476),#4842,.F.);
#5050=ADVANCED_FACE('',(#477),#4843,.F.);
#5051=ADVANCED_FACE('',(#478),#4844,.T.);
#5052=ADVANCED_FACE('',(#479),#4845,.T.);
#5053=ADVANCED_FACE('',(#480),#4846,.F.);
#5054=ADVANCED_FACE('',(#481),#4847,.F.);
#5055=ADVANCED_FACE('',(#482),#4848,.T.);
#5056=ADVANCED_FACE('',(#483),#188,.T.);
#5057=ADVANCED_FACE('',(#484),#189,.T.);
#5058=ADVANCED_FACE('',(#485),#190,.T.);
#5059=ADVANCED_FACE('',(#486),#191,.T.);
#5060=ADVANCED_FACE('',(#487),#192,.T.);
#5061=ADVANCED_FACE('',(#488),#193,.T.);
#5062=ADVANCED_FACE('',(#489),#194,.T.);
#5063=ADVANCED_FACE('',(#490),#195,.T.);
#5064=ADVANCED_FACE('',(#491),#196,.T.);
#5065=ADVANCED_FACE('',(#492),#197,.T.);
#5066=ADVANCED_FACE('',(#493),#198,.T.);
#5067=ADVANCED_FACE('',(#494),#199,.T.);
#5068=ADVANCED_FACE('',(#495),#200,.T.);
#5069=ADVANCED_FACE('',(#496),#201,.T.);
#5070=ADVANCED_FACE('',(#497),#202,.T.);
#5071=ADVANCED_FACE('',(#498),#203,.T.);
#5072=ADVANCED_FACE('',(#499),#204,.F.);
#5073=ADVANCED_FACE('',(#500),#4849,.T.);
#5074=ADVANCED_FACE('',(#501),#4850,.T.);
#5075=ADVANCED_FACE('',(#502),#4851,.T.);
#5076=ADVANCED_FACE('',(#503,#284,#285),#4852,.F.);
#5077=ADVANCED_FACE('',(#504),#4853,.F.);
#5078=ADVANCED_FACE('',(#505),#205,.F.);
#5079=ADVANCED_FACE('',(#506),#4854,.T.);
#5080=ADVANCED_FACE('',(#507),#206,.F.);
#5081=ADVANCED_FACE('',(#508,#286,#287),#4855,.F.);
#5082=ADVANCED_FACE('',(#509),#4856,.F.);
#5083=ADVANCED_FACE('',(#510),#4857,.F.);
#5084=ADVANCED_FACE('',(#511),#207,.T.);
#5085=ADVANCED_FACE('',(#512),#208,.T.);
#5086=ADVANCED_FACE('',(#513),#209,.T.);
#5087=ADVANCED_FACE('',(#514),#210,.T.);
#5088=ADVANCED_FACE('',(#515),#4858,.T.);
#5089=ADVANCED_FACE('',(#516),#211,.F.);
#5090=ADVANCED_FACE('',(#517),#212,.F.);
#5091=ADVANCED_FACE('',(#518),#213,.T.);
#5092=ADVANCED_FACE('',(#519),#214,.F.);
#5093=ADVANCED_FACE('',(#520),#215,.T.);
#5094=ADVANCED_FACE('',(#521),#216,.F.);
#5095=ADVANCED_FACE('',(#522),#217,.T.);
#5096=ADVANCED_FACE('',(#523),#4859,.T.);
#5097=ADVANCED_FACE('',(#524),#4860,.F.);
#5098=ADVANCED_FACE('',(#525),#109,.T.);
#5099=ADVANCED_FACE('',(#526),#110,.T.);
#5100=ADVANCED_FACE('',(#527,#288),#4861,.T.);
#5101=ADVANCED_FACE('',(#528),#218,.T.);
#5102=ADVANCED_FACE('',(#529,#289),#4862,.T.);
#5103=ADVANCED_FACE('',(#530),#219,.F.);
#5104=ADVANCED_FACE('',(#531),#99,.F.);
#5105=ADVANCED_FACE('',(#532,#290),#4863,.T.);
#5106=ADVANCED_FACE('',(#533),#220,.F.);
#5107=ADVANCED_FACE('',(#534),#100,.T.);
#5108=ADVANCED_FACE('',(#535),#221,.T.);
#5109=ADVANCED_FACE('',(#536),#101,.F.);
#5110=ADVANCED_FACE('',(#537,#291),#4864,.T.);
#5111=ADVANCED_FACE('',(#538),#222,.F.);
#5112=ADVANCED_FACE('',(#539),#102,.T.);
#5113=ADVANCED_FACE('',(#540),#223,.T.);
#5114=ADVANCED_FACE('',(#541,#292),#4865,.T.);
#5115=ADVANCED_FACE('',(#542),#224,.F.);
#5116=ADVANCED_FACE('',(#543,#293),#4866,.T.);
#5117=ADVANCED_FACE('',(#544),#225,.F.);
#5118=ADVANCED_FACE('',(#545),#103,.F.);
#5119=ADVANCED_FACE('',(#546),#226,.F.);
#5120=ADVANCED_FACE('',(#547),#104,.F.);
#5121=ADVANCED_FACE('',(#548),#227,.F.);
#5122=ADVANCED_FACE('',(#549,#294),#4867,.T.);
#5123=ADVANCED_FACE('',(#550),#228,.F.);
#5124=ADVANCED_FACE('',(#551,#295),#4868,.T.);
#5125=ADVANCED_FACE('',(#552,#296),#4869,.T.);
#5126=ADVANCED_FACE('',(#553),#229,.T.);
#5127=ADVANCED_FACE('',(#554,#297),#4870,.T.);
#5128=ADVANCED_FACE('',(#555),#230,.T.);
#5129=ADVANCED_FACE('',(#556,#298),#4871,.T.);
#5130=ADVANCED_FACE('',(#557),#231,.T.);
#5131=ADVANCED_FACE('',(#558,#299),#4872,.T.);
#5132=ADVANCED_FACE('',(#559,#300),#4873,.T.);
#5133=ADVANCED_FACE('',(#560),#232,.T.);
#5134=ADVANCED_FACE('',(#561,#301),#4874,.T.);
#5135=ADVANCED_FACE('',(#562),#105,.F.);
#5136=ADVANCED_FACE('',(#563),#233,.F.);
#5137=ADVANCED_FACE('',(#564,#302),#4875,.T.);
#5138=ADVANCED_FACE('',(#565),#106,.T.);
#5139=ADVANCED_FACE('',(#566,#303),#4876,.F.);
#5140=ADVANCED_FACE('',(#567),#234,.T.);
#5141=ADVANCED_FACE('',(#568,#304),#4877,.F.);
#5142=ADVANCED_FACE('',(#569),#235,.F.);
#5143=ADVANCED_FACE('',(#570,#305),#4878,.F.);
#5144=ADVANCED_FACE('',(#571),#236,.T.);
#5145=ADVANCED_FACE('',(#572,#306),#4879,.F.);
#5146=ADVANCED_FACE('',(#573),#107,.F.);
#5147=ADVANCED_FACE('',(#574),#237,.F.);
#5148=ADVANCED_FACE('',(#575,#307),#4880,.F.);
#5149=ADVANCED_FACE('',(#576),#108,.T.);
#5150=CLOSED_SHELL('',(#4881,#4882,#4883,#4884,#4885,#4886,#4887,#4888,
#4889,#4890,#4891,#4892,#4893,#4894,#4895,#4896,#4897,#4898,#4899,#4900,
#4901,#4902));
#5151=CLOSED_SHELL('',(#4903,#4904,#4905,#4906,#4907,#4908,#4909,#4910,
#4911,#4912,#4913,#4914,#4915,#4916,#4917,#4918,#4919,#4920,#4921,#4922,
#4923,#4924,#4925,#4926,#4927,#4928,#4929,#4930,#4931,#4932,#4933,#4934,
#4935,#4936,#4937,#4938,#4939,#4940,#4941,#4942,#4943,#4944,#4945,#4946,
#4947,#4948,#4949,#4950,#4951,#4952,#4953,#4954,#4955,#4956,#4957,#4958,
#4959,#4960,#4961,#4962,#4963,#4964,#4965,#4966,#4967,#4968,#4969,#4970,
#4971,#4972,#4973,#4974,#4975,#4976,#4977,#4978,#4979,#4980,#4981,#4982,
#4983,#4984,#4985,#4986,#4987,#4988,#4989,#4990,#4991,#4992,#4993,#4994,
#4995,#4996,#4997,#4998,#4999,#5000,#5001,#5002,#5003,#5004,#5005,#5006,
#5007,#5008,#5009,#5010,#5011,#5012,#5013,#5014,#5015,#5016,#5017,#5018,
#5019,#5020,#5021,#5022,#5023,#5024,#5025,#5026,#5027,#5028,#5029,#5030,
#5031,#5032,#5033,#5034,#5035,#5036,#5037,#5038,#5039,#5040,#5041,#5042,
#5043,#5044,#5045,#5046,#5047,#5048,#5049,#5050,#5051,#5052,#5053,#5054,
#5055,#5056,#5057,#5058,#5059,#5060,#5061,#5062,#5063,#5064,#5065,#5066,
#5067,#5068,#5069,#5070,#5071,#5072));
#5152=CLOSED_SHELL('',(#5073,#5074,#5075,#5076,#5077,#5078,#5079,#5080,
#5081,#5082,#5083,#5084,#5085,#5086,#5087,#5088,#5089,#5090,#5091,#5092,
#5093,#5094));
#5153=CLOSED_SHELL('',(#5095,#5096,#5097,#5098,#5099));
#5154=CLOSED_SHELL('',(#5100,#5101,#5102,#5103));
#5155=CLOSED_SHELL('',(#5104,#5105,#5106,#5107,#5108,#5109,#5110,#5111,
#5112,#5113,#5114,#5115,#5116,#5117,#5118,#5119,#5120,#5121,#5122,#5123,
#5124,#5125,#5126,#5127,#5128,#5129,#5130,#5131));
#5156=CLOSED_SHELL('',(#5132,#5133,#5134,#5135,#5136,#5137,#5138));
#5157=CLOSED_SHELL('',(#5139,#5140,#5141,#5142));
#5158=CLOSED_SHELL('',(#5143,#5144,#5145,#5146,#5147,#5148,#5149));
#5159=DERIVED_UNIT_ELEMENT(#5177,1.);
#5160=DERIVED_UNIT_ELEMENT(#8945,-3.);
#5161=DERIVED_UNIT_ELEMENT(#5177,1.);
#5162=DERIVED_UNIT_ELEMENT(#8945,-3.);
#5163=DERIVED_UNIT_ELEMENT(#5177,1.);
#5164=DERIVED_UNIT_ELEMENT(#8945,-3.);
#5165=DERIVED_UNIT_ELEMENT(#5177,1.);
#5166=DERIVED_UNIT_ELEMENT(#8945,-3.);
#5167=DERIVED_UNIT_ELEMENT(#5177,1.);
#5168=DERIVED_UNIT_ELEMENT(#8945,-3.);
#5169=DERIVED_UNIT_ELEMENT(#5177,1.);
#5170=DERIVED_UNIT_ELEMENT(#8945,-3.);
#5171=DERIVED_UNIT_ELEMENT(#5177,1.);
#5172=DERIVED_UNIT_ELEMENT(#8945,-3.);
#5173=DERIVED_UNIT_ELEMENT(#5177,1.);
#5174=DERIVED_UNIT_ELEMENT(#8945,-3.);
#5175=DERIVED_UNIT_ELEMENT(#5177,1.);
#5176=DERIVED_UNIT_ELEMENT(#8945,-3.);
#5177=(
MASS_UNIT()
NAMED_UNIT(*)
SI_UNIT(.KILO.,.GRAM.)
);
#5178=DERIVED_UNIT((#5159,#5160));
#5179=DERIVED_UNIT((#5161,#5162));
#5180=DERIVED_UNIT((#5163,#5164));
#5181=DERIVED_UNIT((#5165,#5166));
#5182=DERIVED_UNIT((#5167,#5168));
#5183=DERIVED_UNIT((#5169,#5170));
#5184=DERIVED_UNIT((#5171,#5172));
#5185=DERIVED_UNIT((#5173,#5174));
#5186=DERIVED_UNIT((#5175,#5176));
#5187=MEASURE_REPRESENTATION_ITEM('density measure',
POSITIVE_RATIO_MEASURE(7850.),#5178);
#5188=MEASURE_REPRESENTATION_ITEM('density measure',
POSITIVE_RATIO_MEASURE(7850.),#5179);
#5189=MEASURE_REPRESENTATION_ITEM('density measure',
POSITIVE_RATIO_MEASURE(7850.),#5180);
#5190=MEASURE_REPRESENTATION_ITEM('density measure',
POSITIVE_RATIO_MEASURE(7850.),#5181);
#5191=MEASURE_REPRESENTATION_ITEM('density measure',
POSITIVE_RATIO_MEASURE(7850.),#5182);
#5192=MEASURE_REPRESENTATION_ITEM('density measure',
POSITIVE_RATIO_MEASURE(7850.),#5183);
#5193=MEASURE_REPRESENTATION_ITEM('density measure',
POSITIVE_RATIO_MEASURE(7850.),#5184);
#5194=MEASURE_REPRESENTATION_ITEM('density measure',
POSITIVE_RATIO_MEASURE(7850.),#5185);
#5195=MEASURE_REPRESENTATION_ITEM('density measure',
POSITIVE_RATIO_MEASURE(7850.),#5186);
#5196=PROPERTY_DEFINITION_REPRESENTATION(#5241,#5214);
#5197=PROPERTY_DEFINITION_REPRESENTATION(#5242,#5215);
#5198=PROPERTY_DEFINITION_REPRESENTATION(#5243,#5216);
#5199=PROPERTY_DEFINITION_REPRESENTATION(#5244,#5217);
#5200=PROPERTY_DEFINITION_REPRESENTATION(#5245,#5218);
#5201=PROPERTY_DEFINITION_REPRESENTATION(#5246,#5219);
#5202=PROPERTY_DEFINITION_REPRESENTATION(#5247,#5220);
#5203=PROPERTY_DEFINITION_REPRESENTATION(#5248,#5221);
#5204=PROPERTY_DEFINITION_REPRESENTATION(#5249,#5222);
#5205=PROPERTY_DEFINITION_REPRESENTATION(#5250,#5223);
#5206=PROPERTY_DEFINITION_REPRESENTATION(#5251,#5224);
#5207=PROPERTY_DEFINITION_REPRESENTATION(#5252,#5225);
#5208=PROPERTY_DEFINITION_REPRESENTATION(#5253,#5226);
#5209=PROPERTY_DEFINITION_REPRESENTATION(#5254,#5227);
#5210=PROPERTY_DEFINITION_REPRESENTATION(#5255,#5228);
#5211=PROPERTY_DEFINITION_REPRESENTATION(#5256,#5229);
#5212=PROPERTY_DEFINITION_REPRESENTATION(#5257,#5230);
#5213=PROPERTY_DEFINITION_REPRESENTATION(#5258,#5231);
#5214=REPRESENTATION('material name',(#5232),#8934);
#5215=REPRESENTATION('density',(#5187),#8934);
#5216=REPRESENTATION('material name',(#5233),#8935);
#5217=REPRESENTATION('density',(#5188),#8935);
#5218=REPRESENTATION('material name',(#5234),#8936);
#5219=REPRESENTATION('density',(#5189),#8936);
#5220=REPRESENTATION('material name',(#5235),#8937);
#5221=REPRESENTATION('density',(#5190),#8937);
#5222=REPRESENTATION('material name',(#5236),#8939);
#5223=REPRESENTATION('density',(#5191),#8939);
#5224=REPRESENTATION('material name',(#5237),#8940);
#5225=REPRESENTATION('density',(#5192),#8940);
#5226=REPRESENTATION('material name',(#5238),#8941);
#5227=REPRESENTATION('density',(#5193),#8941);
#5228=REPRESENTATION('material name',(#5239),#8942);
#5229=REPRESENTATION('density',(#5194),#8942);
#5230=REPRESENTATION('material name',(#5240),#8943);
#5231=REPRESENTATION('density',(#5195),#8943);
#5232=DESCRIPTIVE_REPRESENTATION_ITEM('Steel','Steel');
#5233=DESCRIPTIVE_REPRESENTATION_ITEM('Steel','Steel');
#5234=DESCRIPTIVE_REPRESENTATION_ITEM('Steel','Steel');
#5235=DESCRIPTIVE_REPRESENTATION_ITEM('Steel','Steel');
#5236=DESCRIPTIVE_REPRESENTATION_ITEM('Steel','Steel');
#5237=DESCRIPTIVE_REPRESENTATION_ITEM('Steel','Steel');
#5238=DESCRIPTIVE_REPRESENTATION_ITEM('Steel','Steel');
#5239=DESCRIPTIVE_REPRESENTATION_ITEM('Steel','Steel');
#5240=DESCRIPTIVE_REPRESENTATION_ITEM('Steel','Steel');
#5241=PROPERTY_DEFINITION('material property','material name',#9005);
#5242=PROPERTY_DEFINITION('material property','density of part',#9005);
#5243=PROPERTY_DEFINITION('material property','material name',#9006);
#5244=PROPERTY_DEFINITION('material property','density of part',#9006);
#5245=PROPERTY_DEFINITION('material property','material name',#9007);
#5246=PROPERTY_DEFINITION('material property','density of part',#9007);
#5247=PROPERTY_DEFINITION('material property','material name',#9008);
#5248=PROPERTY_DEFINITION('material property','density of part',#9008);
#5249=PROPERTY_DEFINITION('material property','material name',#9010);
#5250=PROPERTY_DEFINITION('material property','density of part',#9010);
#5251=PROPERTY_DEFINITION('material property','material name',#9011);
#5252=PROPERTY_DEFINITION('material property','density of part',#9011);
#5253=PROPERTY_DEFINITION('material property','material name',#9012);
#5254=PROPERTY_DEFINITION('material property','density of part',#9012);
#5255=PROPERTY_DEFINITION('material property','material name',#9013);
#5256=PROPERTY_DEFINITION('material property','density of part',#9013);
#5257=PROPERTY_DEFINITION('material property','material name',#9014);
#5258=PROPERTY_DEFINITION('material property','density of part',#9014);
#5259=AXIS2_PLACEMENT_3D('',#7388,#5817,#5818);
#5260=AXIS2_PLACEMENT_3D('',#7389,#5819,#5820);
#5261=AXIS2_PLACEMENT_3D('',#7390,#5821,#5822);
#5262=AXIS2_PLACEMENT_3D('',#7395,#5824,#5825);
#5263=AXIS2_PLACEMENT_3D('',#7399,#5827,#5828);
#5264=AXIS2_PLACEMENT_3D('',#7403,#5830,#5831);
#5265=AXIS2_PLACEMENT_3D('',#7407,#5833,#5834);
#5266=AXIS2_PLACEMENT_3D('',#7411,#5836,#5837);
#5267=AXIS2_PLACEMENT_3D('',#7413,#5838,#5839);
#5268=AXIS2_PLACEMENT_3D('',#7417,#5841,#5842);
#5269=AXIS2_PLACEMENT_3D('',#7418,#5843,#5844);
#5270=AXIS2_PLACEMENT_3D('',#7419,#5845,#5846);
#5271=AXIS2_PLACEMENT_3D('',#7425,#5850,#5851);
#5272=AXIS2_PLACEMENT_3D('',#7431,#5855,#5856);
#5273=AXIS2_PLACEMENT_3D('',#7438,#5860,#5861);
#5274=AXIS2_PLACEMENT_3D('',#7440,#5862,#5863);
#5275=AXIS2_PLACEMENT_3D('',#7441,#5864,#5865);
#5276=AXIS2_PLACEMENT_3D('',#7447,#5869,#5870);
#5277=AXIS2_PLACEMENT_3D('',#7449,#5871,#5872);
#5278=AXIS2_PLACEMENT_3D('',#7452,#5874,#5875);
#5279=AXIS2_PLACEMENT_3D('',#7453,#5876,#5877);
#5280=AXIS2_PLACEMENT_3D('',#7459,#5881,#5882);
#5281=AXIS2_PLACEMENT_3D('',#7461,#5883,#5884);
#5282=AXIS2_PLACEMENT_3D('',#7464,#5886,#5887);
#5283=AXIS2_PLACEMENT_3D('',#7465,#5888,#5889);
#5284=AXIS2_PLACEMENT_3D('',#7470,#5891,#5892);
#5285=AXIS2_PLACEMENT_3D('',#7471,#5893,#5894);
#5286=AXIS2_PLACEMENT_3D('',#7472,#5895,#5896);
#5287=AXIS2_PLACEMENT_3D('',#7473,#5897,#5898);
#5288=AXIS2_PLACEMENT_3D('',#7474,#5899,#5900);
#5289=AXIS2_PLACEMENT_3D('',#7475,#5901,#5902);
#5290=AXIS2_PLACEMENT_3D('',#7477,#5903,#5904);
#5291=AXIS2_PLACEMENT_3D('',#7478,#5905,#5906);
#5292=AXIS2_PLACEMENT_3D('',#7479,#5907,#5908);
#5293=AXIS2_PLACEMENT_3D('',#7480,#5909,#5910);
#5294=AXIS2_PLACEMENT_3D('',#7481,#5911,#5912);
#5295=AXIS2_PLACEMENT_3D('',#7482,#5913,#5914);
#5296=AXIS2_PLACEMENT_3D('',#7483,#5915,#5916);
#5297=AXIS2_PLACEMENT_3D('',#7484,#5917,#5918);
#5298=AXIS2_PLACEMENT_3D('',#7485,#5919,#5920);
#5299=AXIS2_PLACEMENT_3D('',#7489,#5922,#5923);
#5300=AXIS2_PLACEMENT_3D('',#7491,#5924,#5925);
#5301=AXIS2_PLACEMENT_3D('',#7496,#5928,#5929);
#5302=AXIS2_PLACEMENT_3D('',#7498,#5931,#5932);
#5303=AXIS2_PLACEMENT_3D('',#7513,#5934,#5935);
#5304=AXIS2_PLACEMENT_3D('',#7525,#5937,#5938);
#5305=AXIS2_PLACEMENT_3D('',#7527,#5940,#5941);
#5306=AXIS2_PLACEMENT_3D('',#7528,#5942,#5943);
#5307=AXIS2_PLACEMENT_3D('',#7530,#5945,#5946);
#5308=AXIS2_PLACEMENT_3D('',#7531,#5947,#5948);
#5309=AXIS2_PLACEMENT_3D('',#7532,#5949,#5950);
#5310=AXIS2_PLACEMENT_3D('',#7541,#5955,#5956);
#5311=AXIS2_PLACEMENT_3D('',#7550,#5961,#5962);
#5312=AXIS2_PLACEMENT_3D('',#7553,#5965,#5966);
#5313=AXIS2_PLACEMENT_3D('',#7567,#5974,#5975);
#5314=AXIS2_PLACEMENT_3D('',#7581,#5983,#5984);
#5315=AXIS2_PLACEMENT_3D('',#7587,#5988,#5989);
#5316=AXIS2_PLACEMENT_3D('',#7596,#5994,#5995);
#5317=AXIS2_PLACEMENT_3D('',#7602,#5999,#6000);
#5318=AXIS2_PLACEMENT_3D('',#7608,#6004,#6005);
#5319=AXIS2_PLACEMENT_3D('',#7676,#6040,#6041);
#5320=AXIS2_PLACEMENT_3D('',#7679,#6042,#6043);
#5321=AXIS2_PLACEMENT_3D('',#7683,#6046,#6047);
#5322=AXIS2_PLACEMENT_3D('',#7688,#6049,#6050);
#5323=AXIS2_PLACEMENT_3D('',#7690,#6052,#6053);
#5324=AXIS2_PLACEMENT_3D('',#7693,#6054,#6055);
#5325=AXIS2_PLACEMENT_3D('',#7697,#6058,#6059);
#5326=AXIS2_PLACEMENT_3D('',#7702,#6061,#6062);
#5327=AXIS2_PLACEMENT_3D('',#7704,#6064,#6065);
#5328=AXIS2_PLACEMENT_3D('',#7707,#6066,#6067);
#5329=AXIS2_PLACEMENT_3D('',#7711,#6070,#6071);
#5330=AXIS2_PLACEMENT_3D('',#7714,#6072,#6073);
#5331=AXIS2_PLACEMENT_3D('',#7718,#6076,#6077);
#5332=AXIS2_PLACEMENT_3D('',#7724,#6081,#6082);
#5333=AXIS2_PLACEMENT_3D('',#7729,#6084,#6085);
#5334=AXIS2_PLACEMENT_3D('',#7731,#6087,#6088);
#5335=AXIS2_PLACEMENT_3D('',#7734,#6089,#6090);
#5336=AXIS2_PLACEMENT_3D('',#7738,#6093,#6094);
#5337=AXIS2_PLACEMENT_3D('',#7743,#6096,#6097);
#5338=AXIS2_PLACEMENT_3D('',#7745,#6099,#6100);
#5339=AXIS2_PLACEMENT_3D('',#7763,#6113,#6114);
#5340=AXIS2_PLACEMENT_3D('',#7766,#6117,#6118);
#5341=AXIS2_PLACEMENT_3D('',#7834,#6153,#6154);
#5342=AXIS2_PLACEMENT_3D('',#7837,#6155,#6156);
#5343=AXIS2_PLACEMENT_3D('',#7841,#6159,#6160);
#5344=AXIS2_PLACEMENT_3D('',#7846,#6162,#6163);
#5345=AXIS2_PLACEMENT_3D('',#7848,#6165,#6166);
#5346=AXIS2_PLACEMENT_3D('',#7853,#6168,#6169);
#5347=AXIS2_PLACEMENT_3D('',#7855,#6171,#6172);
#5348=AXIS2_PLACEMENT_3D('',#7864,#6177,#6178);
#5349=AXIS2_PLACEMENT_3D('',#7873,#6183,#6184);
#5350=AXIS2_PLACEMENT_3D('',#7882,#6189,#6190);
#5351=AXIS2_PLACEMENT_3D('',#7885,#6191,#6192);
#5352=AXIS2_PLACEMENT_3D('',#7889,#6195,#6196);
#5353=AXIS2_PLACEMENT_3D('',#7894,#6198,#6199);
#5354=AXIS2_PLACEMENT_3D('',#7896,#6201,#6202);
#5355=AXIS2_PLACEMENT_3D('',#7905,#6207,#6208);
#5356=AXIS2_PLACEMENT_3D('',#7908,#6211,#6212);
#5357=AXIS2_PLACEMENT_3D('',#7914,#6216,#6217);
#5358=AXIS2_PLACEMENT_3D('',#7917,#6220,#6221);
#5359=AXIS2_PLACEMENT_3D('',#7946,#6238,#6239);
#5360=AXIS2_PLACEMENT_3D('',#7952,#6243,#6244);
#5361=AXIS2_PLACEMENT_3D('',#7959,#6249,#6250);
#5362=AXIS2_PLACEMENT_3D('',#7961,#6251,#6252);
#5363=AXIS2_PLACEMENT_3D('',#7969,#6257,#6258);
#5364=AXIS2_PLACEMENT_3D('',#7974,#6261,#6262);
#5365=AXIS2_PLACEMENT_3D('',#7976,#6264,#6265);
#5366=AXIS2_PLACEMENT_3D('',#7979,#6267,#6268);
#5367=AXIS2_PLACEMENT_3D('',#7981,#6269,#6270);
#5368=AXIS2_PLACEMENT_3D('',#7983,#6271,#6272);
#5369=AXIS2_PLACEMENT_3D('',#7985,#6273,#6274);
#5370=AXIS2_PLACEMENT_3D('',#7987,#6275,#6276);
#5371=AXIS2_PLACEMENT_3D('',#7988,#6277,#6278);
#5372=AXIS2_PLACEMENT_3D('',#7991,#6280,#6281);
#5373=AXIS2_PLACEMENT_3D('',#7993,#6282,#6283);
#5374=AXIS2_PLACEMENT_3D('',#7998,#6286,#6287);
#5375=AXIS2_PLACEMENT_3D('',#7999,#6288,#6289);
#5376=AXIS2_PLACEMENT_3D('',#8001,#6290,#6291);
#5377=AXIS2_PLACEMENT_3D('',#8003,#6292,#6293);
#5378=AXIS2_PLACEMENT_3D('',#8005,#6294,#6295);
#5379=AXIS2_PLACEMENT_3D('',#8007,#6296,#6297);
#5380=AXIS2_PLACEMENT_3D('',#8009,#6298,#6299);
#5381=AXIS2_PLACEMENT_3D('',#8010,#6300,#6301);
#5382=AXIS2_PLACEMENT_3D('',#8012,#6303,#6304);
#5383=AXIS2_PLACEMENT_3D('',#8014,#6306,#6307);
#5384=AXIS2_PLACEMENT_3D('',#8015,#6308,#6309);
#5385=AXIS2_PLACEMENT_3D('',#8017,#6311,#6312);
#5386=AXIS2_PLACEMENT_3D('',#8019,#6314,#6315);
#5387=AXIS2_PLACEMENT_3D('',#8021,#6317,#6318);
#5388=AXIS2_PLACEMENT_3D('',#8023,#6320,#6321);
#5389=AXIS2_PLACEMENT_3D('',#8025,#6323,#6324);
#5390=AXIS2_PLACEMENT_3D('',#8028,#6327,#6328);
#5391=AXIS2_PLACEMENT_3D('',#8030,#6329,#6330);
#5392=AXIS2_PLACEMENT_3D('',#8032,#6332,#6333);
#5393=AXIS2_PLACEMENT_3D('',#8033,#6334,#6335);
#5394=AXIS2_PLACEMENT_3D('',#8034,#6336,#6337);
#5395=AXIS2_PLACEMENT_3D('',#8035,#6338,#6339);
#5396=AXIS2_PLACEMENT_3D('',#8036,#6340,#6341);
#5397=AXIS2_PLACEMENT_3D('',#8037,#6342,#6343);
#5398=AXIS2_PLACEMENT_3D('',#8038,#6344,#6345);
#5399=AXIS2_PLACEMENT_3D('',#8039,#6346,#6347);
#5400=AXIS2_PLACEMENT_3D('',#8040,#6348,#6349);
#5401=AXIS2_PLACEMENT_3D('',#8043,#6350,#6351);
#5402=AXIS2_PLACEMENT_3D('',#8047,#6354,#6355);
#5403=AXIS2_PLACEMENT_3D('',#8053,#6359,#6360);
#5404=AXIS2_PLACEMENT_3D('',#8055,#6361,#6362);
#5405=AXIS2_PLACEMENT_3D('',#8057,#6364,#6365);
#5406=AXIS2_PLACEMENT_3D('',#8058,#6366,#6367);
#5407=AXIS2_PLACEMENT_3D('',#8059,#6368,#6369);
#5408=AXIS2_PLACEMENT_3D('',#8060,#6370,#6371);
#5409=AXIS2_PLACEMENT_3D('',#8061,#6372,#6373);
#5410=AXIS2_PLACEMENT_3D('',#8062,#6374,#6375);
#5411=AXIS2_PLACEMENT_3D('',#8063,#6376,#6377);
#5412=AXIS2_PLACEMENT_3D('',#8064,#6378,#6379);
#5413=AXIS2_PLACEMENT_3D('',#8065,#6380,#6381);
#5414=AXIS2_PLACEMENT_3D('',#8071,#6387,#6388);
#5415=AXIS2_PLACEMENT_3D('',#8074,#6389,#6390);
#5416=AXIS2_PLACEMENT_3D('',#8078,#6392,#6393);
#5417=AXIS2_PLACEMENT_3D('',#8082,#6395,#6396);
#5418=AXIS2_PLACEMENT_3D('',#8086,#6398,#6399);
#5419=AXIS2_PLACEMENT_3D('',#8092,#6402,#6403);
#5420=AXIS2_PLACEMENT_3D('',#8095,#6405,#6406);
#5421=AXIS2_PLACEMENT_3D('',#8100,#6408,#6409);
#5422=AXIS2_PLACEMENT_3D('',#8103,#6411,#6412);
#5423=AXIS2_PLACEMENT_3D('',#8108,#6414,#6415);
#5424=AXIS2_PLACEMENT_3D('',#8111,#6417,#6418);
#5425=AXIS2_PLACEMENT_3D('',#8116,#6420,#6421);
#5426=AXIS2_PLACEMENT_3D('',#8119,#6423,#6424);
#5427=AXIS2_PLACEMENT_3D('',#8122,#6425,#6426);
#5428=AXIS2_PLACEMENT_3D('',#8126,#6428,#6429);
#5429=AXIS2_PLACEMENT_3D('',#8132,#6432,#6433);
#5430=AXIS2_PLACEMENT_3D('',#8135,#6435,#6436);
#5431=AXIS2_PLACEMENT_3D('',#8136,#6437,#6438);
#5432=AXIS2_PLACEMENT_3D('',#8138,#6439,#6440);
#5433=AXIS2_PLACEMENT_3D('',#8139,#6441,#6442);
#5434=AXIS2_PLACEMENT_3D('',#8141,#6444,#6445);
#5435=AXIS2_PLACEMENT_3D('',#8143,#6447,#6448);
#5436=AXIS2_PLACEMENT_3D('',#8145,#6449,#6450);
#5437=AXIS2_PLACEMENT_3D('',#8146,#6451,#6452);
#5438=AXIS2_PLACEMENT_3D('',#8147,#6453,#6454);
#5439=AXIS2_PLACEMENT_3D('',#8150,#6457,#6458);
#5440=AXIS2_PLACEMENT_3D('',#8152,#6459,#6460);
#5441=AXIS2_PLACEMENT_3D('',#8153,#6461,#6462);
#5442=AXIS2_PLACEMENT_3D('',#8154,#6463,#6464);
#5443=AXIS2_PLACEMENT_3D('',#8156,#6465,#6466);
#5444=AXIS2_PLACEMENT_3D('',#8157,#6467,#6468);
#5445=AXIS2_PLACEMENT_3D('',#8158,#6469,#6470);
#5446=AXIS2_PLACEMENT_3D('',#8160,#6471,#6472);
#5447=AXIS2_PLACEMENT_3D('',#8161,#6473,#6474);
#5448=AXIS2_PLACEMENT_3D('',#8163,#6476,#6477);
#5449=AXIS2_PLACEMENT_3D('',#8165,#6479,#6480);
#5450=AXIS2_PLACEMENT_3D('',#8167,#6481,#6482);
#5451=AXIS2_PLACEMENT_3D('',#8168,#6483,#6484);
#5452=AXIS2_PLACEMENT_3D('',#8169,#6485,#6486);
#5453=AXIS2_PLACEMENT_3D('',#8171,#6487,#6488);
#5454=AXIS2_PLACEMENT_3D('',#8172,#6489,#6490);
#5455=AXIS2_PLACEMENT_3D('',#8174,#6492,#6493);
#5456=AXIS2_PLACEMENT_3D('',#8176,#6495,#6496);
#5457=AXIS2_PLACEMENT_3D('',#8178,#6497,#6498);
#5458=AXIS2_PLACEMENT_3D('',#8179,#6499,#6500);
#5459=AXIS2_PLACEMENT_3D('',#8180,#6501,#6502);
#5460=AXIS2_PLACEMENT_3D('',#8182,#6503,#6504);
#5461=AXIS2_PLACEMENT_3D('',#8183,#6505,#6506);
#5462=AXIS2_PLACEMENT_3D('',#8185,#6508,#6509);
#5463=AXIS2_PLACEMENT_3D('',#8187,#6511,#6512);
#5464=AXIS2_PLACEMENT_3D('',#8189,#6513,#6514);
#5465=AXIS2_PLACEMENT_3D('',#8190,#6515,#6516);
#5466=AXIS2_PLACEMENT_3D('',#8191,#6517,#6518);
#5467=AXIS2_PLACEMENT_3D('',#8193,#6519,#6520);
#5468=AXIS2_PLACEMENT_3D('',#8194,#6521,#6522);
#5469=AXIS2_PLACEMENT_3D('',#8196,#6524,#6525);
#5470=AXIS2_PLACEMENT_3D('',#8198,#6527,#6528);
#5471=AXIS2_PLACEMENT_3D('',#8200,#6529,#6530);
#5472=AXIS2_PLACEMENT_3D('',#8201,#6531,#6532);
#5473=AXIS2_PLACEMENT_3D('',#8202,#6533,#6534);
#5474=AXIS2_PLACEMENT_3D('',#8205,#6537,#6538);
#5475=AXIS2_PLACEMENT_3D('',#8207,#6539,#6540);
#5476=AXIS2_PLACEMENT_3D('',#8208,#6541,#6542);
#5477=AXIS2_PLACEMENT_3D('',#8209,#6543,#6544);
#5478=AXIS2_PLACEMENT_3D('',#8211,#6545,#6546);
#5479=AXIS2_PLACEMENT_3D('',#8212,#6547,#6548);
#5480=AXIS2_PLACEMENT_3D('',#8213,#6549,#6550);
#5481=AXIS2_PLACEMENT_3D('',#8216,#6553,#6554);
#5482=AXIS2_PLACEMENT_3D('',#8218,#6555,#6556);
#5483=AXIS2_PLACEMENT_3D('',#8219,#6557,#6558);
#5484=AXIS2_PLACEMENT_3D('',#8220,#6559,#6560);
#5485=AXIS2_PLACEMENT_3D('',#8222,#6561,#6562);
#5486=AXIS2_PLACEMENT_3D('',#8223,#6563,#6564);
#5487=AXIS2_PLACEMENT_3D('',#8224,#6565,#6566);
#5488=AXIS2_PLACEMENT_3D('',#8226,#6568,#6569);
#5489=AXIS2_PLACEMENT_3D('',#8227,#6570,#6571);
#5490=AXIS2_PLACEMENT_3D('',#8229,#6573,#6574);
#5491=AXIS2_PLACEMENT_3D('',#8230,#6575,#6576);
#5492=AXIS2_PLACEMENT_3D('',#8232,#6578,#6579);
#5493=AXIS2_PLACEMENT_3D('',#8233,#6580,#6581);
#5494=AXIS2_PLACEMENT_3D('',#8235,#6583,#6584);
#5495=AXIS2_PLACEMENT_3D('',#8236,#6585,#6586);
#5496=AXIS2_PLACEMENT_3D('',#8238,#6588,#6589);
#5497=AXIS2_PLACEMENT_3D('',#8239,#6590,#6591);
#5498=AXIS2_PLACEMENT_3D('',#8241,#6593,#6594);
#5499=AXIS2_PLACEMENT_3D('',#8242,#6595,#6596);
#5500=AXIS2_PLACEMENT_3D('',#8244,#6598,#6599);
#5501=AXIS2_PLACEMENT_3D('',#8245,#6600,#6601);
#5502=AXIS2_PLACEMENT_3D('',#8247,#6603,#6604);
#5503=AXIS2_PLACEMENT_3D('',#8248,#6605,#6606);
#5504=AXIS2_PLACEMENT_3D('',#8251,#6607,#6608);
#5505=AXIS2_PLACEMENT_3D('',#8255,#6611,#6612);
#5506=AXIS2_PLACEMENT_3D('',#8261,#6616,#6617);
#5507=AXIS2_PLACEMENT_3D('',#8263,#6618,#6619);
#5508=AXIS2_PLACEMENT_3D('',#8265,#6621,#6622);
#5509=AXIS2_PLACEMENT_3D('',#8271,#6626,#6627);
#5510=AXIS2_PLACEMENT_3D('',#8273,#6628,#6629);
#5511=AXIS2_PLACEMENT_3D('',#8275,#6631,#6632);
#5512=AXIS2_PLACEMENT_3D('',#8276,#6633,#6634);
#5513=AXIS2_PLACEMENT_3D('',#8277,#6635,#6636);
#5514=AXIS2_PLACEMENT_3D('',#8280,#6637,#6638);
#5515=AXIS2_PLACEMENT_3D('',#8284,#6641,#6642);
#5516=AXIS2_PLACEMENT_3D('',#8287,#6645,#6646);
#5517=AXIS2_PLACEMENT_3D('',#8290,#6647,#6648);
#5518=AXIS2_PLACEMENT_3D('',#8294,#6651,#6652);
#5519=AXIS2_PLACEMENT_3D('',#8300,#6656,#6657);
#5520=AXIS2_PLACEMENT_3D('',#8302,#6658,#6659);
#5521=AXIS2_PLACEMENT_3D('',#8304,#6661,#6662);
#5522=AXIS2_PLACEMENT_3D('',#8306,#6664,#6665);
#5523=AXIS2_PLACEMENT_3D('',#8308,#6667,#6668);
#5524=AXIS2_PLACEMENT_3D('',#8310,#6670,#6671);
#5525=AXIS2_PLACEMENT_3D('',#8316,#6677,#6678);
#5526=AXIS2_PLACEMENT_3D('',#8319,#6679,#6680);
#5527=AXIS2_PLACEMENT_3D('',#8323,#6682,#6683);
#5528=AXIS2_PLACEMENT_3D('',#8329,#6686,#6687);
#5529=AXIS2_PLACEMENT_3D('',#8332,#6689,#6690);
#5530=AXIS2_PLACEMENT_3D('',#8337,#6692,#6693);
#5531=AXIS2_PLACEMENT_3D('',#8340,#6695,#6696);
#5532=AXIS2_PLACEMENT_3D('',#8345,#6698,#6699);
#5533=AXIS2_PLACEMENT_3D('',#8348,#6701,#6702);
#5534=AXIS2_PLACEMENT_3D('',#8353,#6704,#6705);
#5535=AXIS2_PLACEMENT_3D('',#8356,#6707,#6708);
#5536=AXIS2_PLACEMENT_3D('',#8359,#6709,#6710);
#5537=AXIS2_PLACEMENT_3D('',#8363,#6712,#6713);
#5538=AXIS2_PLACEMENT_3D('',#8369,#6716,#6717);
#5539=AXIS2_PLACEMENT_3D('',#8372,#6719,#6720);
#5540=AXIS2_PLACEMENT_3D('',#8375,#6721,#6722);
#5541=AXIS2_PLACEMENT_3D('',#8379,#6724,#6725);
#5542=AXIS2_PLACEMENT_3D('',#8381,#6727,#6728);
#5543=AXIS2_PLACEMENT_3D('',#8384,#6731,#6732);
#5544=AXIS2_PLACEMENT_3D('',#8386,#6733,#6734);
#5545=AXIS2_PLACEMENT_3D('',#8389,#6736,#6737);
#5546=AXIS2_PLACEMENT_3D('',#8390,#6738,#6739);
#5547=AXIS2_PLACEMENT_3D('',#8396,#6743,#6744);
#5548=AXIS2_PLACEMENT_3D('',#8397,#6745,#6746);
#5549=AXIS2_PLACEMENT_3D('',#8398,#6747,#6748);
#5550=AXIS2_PLACEMENT_3D('',#8399,#6749,#6750);
#5551=AXIS2_PLACEMENT_3D('',#8408,#6755,#6756);
#5552=AXIS2_PLACEMENT_3D('',#8409,#6757,#6758);
#5553=AXIS2_PLACEMENT_3D('',#8411,#6760,#6761);
#5554=AXIS2_PLACEMENT_3D('',#8412,#6762,#6763);
#5555=AXIS2_PLACEMENT_3D('',#8414,#6765,#6766);
#5556=AXIS2_PLACEMENT_3D('',#8415,#6767,#6768);
#5557=AXIS2_PLACEMENT_3D('',#8416,#6769,#6770);
#5558=AXIS2_PLACEMENT_3D('',#8417,#6771,#6772);
#5559=AXIS2_PLACEMENT_3D('',#8420,#6775,#6776);
#5560=AXIS2_PLACEMENT_3D('',#8422,#6777,#6778);
#5561=AXIS2_PLACEMENT_3D('',#8425,#6780,#6781);
#5562=AXIS2_PLACEMENT_3D('',#8426,#6782,#6783);
#5563=AXIS2_PLACEMENT_3D('',#8432,#6787,#6788);
#5564=AXIS2_PLACEMENT_3D('',#8433,#6789,#6790);
#5565=AXIS2_PLACEMENT_3D('',#8434,#6791,#6792);
#5566=AXIS2_PLACEMENT_3D('',#8435,#6793,#6794);
#5567=AXIS2_PLACEMENT_3D('',#8444,#6799,#6800);
#5568=AXIS2_PLACEMENT_3D('',#8445,#6801,#6802);
#5569=AXIS2_PLACEMENT_3D('',#8447,#6804,#6805);
#5570=AXIS2_PLACEMENT_3D('',#8448,#6806,#6807);
#5571=AXIS2_PLACEMENT_3D('',#8450,#6809,#6810);
#5572=AXIS2_PLACEMENT_3D('',#8451,#6811,#6812);
#5573=AXIS2_PLACEMENT_3D('',#8452,#6813,#6814);
#5574=AXIS2_PLACEMENT_3D('',#8453,#6815,#6816);
#5575=AXIS2_PLACEMENT_3D('',#8462,#6821,#6822);
#5576=AXIS2_PLACEMENT_3D('',#8463,#6823,#6824);
#5577=AXIS2_PLACEMENT_3D('',#8465,#6826,#6827);
#5578=AXIS2_PLACEMENT_3D('',#8466,#6828,#6829);
#5579=AXIS2_PLACEMENT_3D('',#8468,#6831,#6832);
#5580=AXIS2_PLACEMENT_3D('',#8469,#6833,#6834);
#5581=AXIS2_PLACEMENT_3D('',#8470,#6835,#6836);
#5582=AXIS2_PLACEMENT_3D('',#8471,#6837,#6838);
#5583=AXIS2_PLACEMENT_3D('',#8480,#6843,#6844);
#5584=AXIS2_PLACEMENT_3D('',#8481,#6845,#6846);
#5585=AXIS2_PLACEMENT_3D('',#8483,#6848,#6849);
#5586=AXIS2_PLACEMENT_3D('',#8484,#6850,#6851);
#5587=AXIS2_PLACEMENT_3D('',#8486,#6853,#6854);
#5588=AXIS2_PLACEMENT_3D('',#8487,#6855,#6856);
#5589=AXIS2_PLACEMENT_3D('',#8488,#6857,#6858);
#5590=AXIS2_PLACEMENT_3D('',#8489,#6859,#6860);
#5591=AXIS2_PLACEMENT_3D('',#8498,#6865,#6866);
#5592=AXIS2_PLACEMENT_3D('',#8499,#6867,#6868);
#5593=AXIS2_PLACEMENT_3D('',#8501,#6870,#6871);
#5594=AXIS2_PLACEMENT_3D('',#8502,#6872,#6873);
#5595=AXIS2_PLACEMENT_3D('',#8504,#6875,#6876);
#5596=AXIS2_PLACEMENT_3D('',#8505,#6877,#6878);
#5597=AXIS2_PLACEMENT_3D('',#8506,#6879,#6880);
#5598=AXIS2_PLACEMENT_3D('',#8507,#6881,#6882);
#5599=AXIS2_PLACEMENT_3D('',#8510,#6885,#6886);
#5600=AXIS2_PLACEMENT_3D('',#8512,#6887,#6888);
#5601=AXIS2_PLACEMENT_3D('',#8515,#6890,#6891);
#5602=AXIS2_PLACEMENT_3D('',#8516,#6892,#6893);
#5603=AXIS2_PLACEMENT_3D('',#8522,#6897,#6898);
#5604=AXIS2_PLACEMENT_3D('',#8523,#6899,#6900);
#5605=AXIS2_PLACEMENT_3D('',#8524,#6901,#6902);
#5606=AXIS2_PLACEMENT_3D('',#8525,#6903,#6904);
#5607=AXIS2_PLACEMENT_3D('',#8526,#6905,#6906);
#5608=AXIS2_PLACEMENT_3D('',#8527,#6907,#6908);
#5609=AXIS2_PLACEMENT_3D('',#8528,#6909,#6910);
#5610=AXIS2_PLACEMENT_3D('',#8529,#6911,#6912);
#5611=AXIS2_PLACEMENT_3D('',#8530,#6913,#6914);
#5612=AXIS2_PLACEMENT_3D('',#8531,#6915,#6916);
#5613=AXIS2_PLACEMENT_3D('',#8532,#6917,#6918);
#5614=AXIS2_PLACEMENT_3D('',#8533,#6919,#6920);
#5615=AXIS2_PLACEMENT_3D('',#8534,#6921,#6922);
#5616=AXIS2_PLACEMENT_3D('',#8535,#6923,#6924);
#5617=AXIS2_PLACEMENT_3D('',#8536,#6925,#6926);
#5618=AXIS2_PLACEMENT_3D('',#8537,#6927,#6928);
#5619=AXIS2_PLACEMENT_3D('',#8538,#6929,#6930);
#5620=AXIS2_PLACEMENT_3D('',#8539,#6931,#6932);
#5621=AXIS2_PLACEMENT_3D('',#8540,#6933,#6934);
#5622=AXIS2_PLACEMENT_3D('',#8541,#6935,#6936);
#5623=AXIS2_PLACEMENT_3D('',#8542,#6937,#6938);
#5624=AXIS2_PLACEMENT_3D('',#8543,#6939,#6940);
#5625=AXIS2_PLACEMENT_3D('',#8546,#6941,#6942);
#5626=AXIS2_PLACEMENT_3D('',#8550,#6944,#6945);
#5627=AXIS2_PLACEMENT_3D('',#8554,#6947,#6948);
#5628=AXIS2_PLACEMENT_3D('',#8558,#6950,#6951);
#5629=AXIS2_PLACEMENT_3D('',#8562,#6953,#6954);
#5630=AXIS2_PLACEMENT_3D('',#8564,#6955,#6956);
#5631=AXIS2_PLACEMENT_3D('',#8568,#6958,#6959);
#5632=AXIS2_PLACEMENT_3D('',#8570,#6960,#6961);
#5633=AXIS2_PLACEMENT_3D('',#8572,#6963,#6964);
#5634=AXIS2_PLACEMENT_3D('',#8578,#6968,#6969);
#5635=AXIS2_PLACEMENT_3D('',#8584,#6973,#6974);
#5636=AXIS2_PLACEMENT_3D('',#8591,#6978,#6979);
#5637=AXIS2_PLACEMENT_3D('',#8593,#6980,#6981);
#5638=AXIS2_PLACEMENT_3D('',#8594,#6982,#6983);
#5639=AXIS2_PLACEMENT_3D('',#8600,#6987,#6988);
#5640=AXIS2_PLACEMENT_3D('',#8602,#6989,#6990);
#5641=AXIS2_PLACEMENT_3D('',#8605,#6992,#6993);
#5642=AXIS2_PLACEMENT_3D('',#8606,#6994,#6995);
#5643=AXIS2_PLACEMENT_3D('',#8612,#6999,#7000);
#5644=AXIS2_PLACEMENT_3D('',#8614,#7001,#7002);
#5645=AXIS2_PLACEMENT_3D('',#8617,#7004,#7005);
#5646=AXIS2_PLACEMENT_3D('',#8618,#7006,#7007);
#5647=AXIS2_PLACEMENT_3D('',#8623,#7009,#7010);
#5648=AXIS2_PLACEMENT_3D('',#8624,#7011,#7012);
#5649=AXIS2_PLACEMENT_3D('',#8625,#7013,#7014);
#5650=AXIS2_PLACEMENT_3D('',#8626,#7015,#7016);
#5651=AXIS2_PLACEMENT_3D('',#8627,#7017,#7018);
#5652=AXIS2_PLACEMENT_3D('',#8628,#7019,#7020);
#5653=AXIS2_PLACEMENT_3D('',#8630,#7021,#7022);
#5654=AXIS2_PLACEMENT_3D('',#8631,#7023,#7024);
#5655=AXIS2_PLACEMENT_3D('',#8632,#7025,#7026);
#5656=AXIS2_PLACEMENT_3D('',#8633,#7027,#7028);
#5657=AXIS2_PLACEMENT_3D('',#8634,#7029,#7030);
#5658=AXIS2_PLACEMENT_3D('',#8635,#7031,#7032);
#5659=AXIS2_PLACEMENT_3D('',#8636,#7033,#7034);
#5660=AXIS2_PLACEMENT_3D('',#8637,#7035,#7036);
#5661=AXIS2_PLACEMENT_3D('',#8638,#7037,#7038);
#5662=AXIS2_PLACEMENT_3D('',#8642,#7040,#7041);
#5663=AXIS2_PLACEMENT_3D('',#8647,#7044,#7045);
#5664=AXIS2_PLACEMENT_3D('',#8649,#7046,#7047);
#5665=AXIS2_PLACEMENT_3D('',#8651,#7049,#7050);
#5666=AXIS2_PLACEMENT_3D('',#8666,#7052,#7053);
#5667=AXIS2_PLACEMENT_3D('',#8678,#7055,#7056);
#5668=AXIS2_PLACEMENT_3D('',#8680,#7058,#7059);
#5669=AXIS2_PLACEMENT_3D('',#8681,#7060,#7061);
#5670=AXIS2_PLACEMENT_3D('',#8683,#7063,#7064);
#5671=AXIS2_PLACEMENT_3D('',#8684,#7065,#7066);
#5672=AXIS2_PLACEMENT_3D('',#8685,#7067,#7068);
#5673=AXIS2_PLACEMENT_3D('',#8688,#7069,#7070);
#5674=AXIS2_PLACEMENT_3D('',#8692,#7072,#7073);
#5675=AXIS2_PLACEMENT_3D('',#8693,#7074,#7075);
#5676=AXIS2_PLACEMENT_3D('',#8694,#7076,#7077);
#5677=AXIS2_PLACEMENT_3D('',#8695,#7078,#7079);
#5678=AXIS2_PLACEMENT_3D('',#8697,#7080,#7081);
#5679=AXIS2_PLACEMENT_3D('',#8698,#7082,#7083);
#5680=AXIS2_PLACEMENT_3D('',#8700,#7084,#7085);
#5681=AXIS2_PLACEMENT_3D('',#8701,#7086,#7087);
#5682=AXIS2_PLACEMENT_3D('',#8702,#7088,#7089);
#5683=AXIS2_PLACEMENT_3D('',#8703,#7090,#7091);
#5684=AXIS2_PLACEMENT_3D('',#8704,#7092,#7093);
#5685=AXIS2_PLACEMENT_3D('',#8705,#7094,#7095);
#5686=AXIS2_PLACEMENT_3D('',#8706,#7096,#7097);
#5687=AXIS2_PLACEMENT_3D('',#8707,#7098,#7099);
#5688=AXIS2_PLACEMENT_3D('',#8709,#7100,#7101);
#5689=AXIS2_PLACEMENT_3D('',#8711,#7102,#7103);
#5690=AXIS2_PLACEMENT_3D('',#8712,#7104,#7105);
#5691=AXIS2_PLACEMENT_3D('',#8714,#7106,#7107);
#5692=AXIS2_PLACEMENT_3D('',#8716,#7109,#7110);
#5693=AXIS2_PLACEMENT_3D('',#8718,#7111,#7112);
#5694=AXIS2_PLACEMENT_3D('',#8719,#7113,#7114);
#5695=AXIS2_PLACEMENT_3D('',#8721,#7116,#7117);
#5696=AXIS2_PLACEMENT_3D('',#8722,#7118,#7119);
#5697=AXIS2_PLACEMENT_3D('',#8725,#7120,#7121);
#5698=AXIS2_PLACEMENT_3D('',#8728,#7123,#7124);
#5699=AXIS2_PLACEMENT_3D('',#8729,#7125,#7126);
#5700=AXIS2_PLACEMENT_3D('',#8730,#7127,#7128);
#5701=AXIS2_PLACEMENT_3D('',#8732,#7129,#7130);
#5702=AXIS2_PLACEMENT_3D('',#8733,#7131,#7132);
#5703=AXIS2_PLACEMENT_3D('',#8736,#7134,#7135);
#5704=AXIS2_PLACEMENT_3D('',#8737,#7136,#7137);
#5705=AXIS2_PLACEMENT_3D('',#8740,#7138,#7139);
#5706=AXIS2_PLACEMENT_3D('',#8742,#7141,#7142);
#5707=AXIS2_PLACEMENT_3D('',#8743,#7143,#7144);
#5708=AXIS2_PLACEMENT_3D('',#8745,#7145,#7146);
#5709=AXIS2_PLACEMENT_3D('',#8747,#7148,#7149);
#5710=AXIS2_PLACEMENT_3D('',#8750,#7150,#7151);
#5711=AXIS2_PLACEMENT_3D('',#8753,#7153,#7154);
#5712=AXIS2_PLACEMENT_3D('',#8754,#7155,#7156);
#5713=AXIS2_PLACEMENT_3D('',#8755,#7157,#7158);
#5714=AXIS2_PLACEMENT_3D('',#8757,#7159,#7160);
#5715=AXIS2_PLACEMENT_3D('',#8758,#7161,#7162);
#5716=AXIS2_PLACEMENT_3D('',#8760,#7163,#7164);
#5717=AXIS2_PLACEMENT_3D('',#8762,#7166,#7167);
#5718=AXIS2_PLACEMENT_3D('',#8765,#7168,#7169);
#5719=AXIS2_PLACEMENT_3D('',#8767,#7171,#7172);
#5720=AXIS2_PLACEMENT_3D('',#8768,#7173,#7174);
#5721=AXIS2_PLACEMENT_3D('',#8771,#7176,#7177);
#5722=AXIS2_PLACEMENT_3D('',#8772,#7178,#7179);
#5723=AXIS2_PLACEMENT_3D('',#8774,#7180,#7181);
#5724=AXIS2_PLACEMENT_3D('',#8775,#7182,#7183);
#5725=AXIS2_PLACEMENT_3D('',#8777,#7184,#7185);
#5726=AXIS2_PLACEMENT_3D('',#8779,#7187,#7188);
#5727=AXIS2_PLACEMENT_3D('',#8781,#7189,#7190);
#5728=AXIS2_PLACEMENT_3D('',#8782,#7191,#7192);
#5729=AXIS2_PLACEMENT_3D('',#8784,#7193,#7194);
#5730=AXIS2_PLACEMENT_3D('',#8786,#7196,#7197);
#5731=AXIS2_PLACEMENT_3D('',#8788,#7198,#7199);
#5732=AXIS2_PLACEMENT_3D('',#8790,#7201,#7202);
#5733=AXIS2_PLACEMENT_3D('',#8792,#7203,#7204);
#5734=AXIS2_PLACEMENT_3D('',#8794,#7206,#7207);
#5735=AXIS2_PLACEMENT_3D('',#8797,#7209,#7210);
#5736=AXIS2_PLACEMENT_3D('',#8798,#7211,#7212);
#5737=AXIS2_PLACEMENT_3D('',#8800,#7213,#7214);
#5738=AXIS2_PLACEMENT_3D('',#8802,#7216,#7217);
#5739=AXIS2_PLACEMENT_3D('',#8804,#7218,#7219);
#5740=AXIS2_PLACEMENT_3D('',#8805,#7220,#7221);
#5741=AXIS2_PLACEMENT_3D('',#8807,#7222,#7223);
#5742=AXIS2_PLACEMENT_3D('',#8809,#7225,#7226);
#5743=AXIS2_PLACEMENT_3D('',#8810,#7227,#7228);
#5744=AXIS2_PLACEMENT_3D('',#8812,#7229,#7230);
#5745=AXIS2_PLACEMENT_3D('',#8813,#7231,#7232);
#5746=AXIS2_PLACEMENT_3D('',#8815,#7233,#7234);
#5747=AXIS2_PLACEMENT_3D('',#8817,#7236,#7237);
#5748=AXIS2_PLACEMENT_3D('',#8819,#7238,#7239);
#5749=AXIS2_PLACEMENT_3D('',#8820,#7240,#7241);
#5750=AXIS2_PLACEMENT_3D('',#8822,#7242,#7243);
#5751=AXIS2_PLACEMENT_3D('',#8824,#7245,#7246);
#5752=AXIS2_PLACEMENT_3D('',#8826,#7247,#7248);
#5753=AXIS2_PLACEMENT_3D('',#8827,#7249,#7250);
#5754=AXIS2_PLACEMENT_3D('',#8829,#7251,#7252);
#5755=AXIS2_PLACEMENT_3D('',#8831,#7254,#7255);
#5756=AXIS2_PLACEMENT_3D('',#8832,#7256,#7257);
#5757=AXIS2_PLACEMENT_3D('',#8833,#7258,#7259);
#5758=AXIS2_PLACEMENT_3D('',#8835,#7260,#7261);
#5759=AXIS2_PLACEMENT_3D('',#8837,#7262,#7263);
#5760=AXIS2_PLACEMENT_3D('',#8838,#7264,#7265);
#5761=AXIS2_PLACEMENT_3D('',#8840,#7266,#7267);
#5762=AXIS2_PLACEMENT_3D('',#8842,#7269,#7270);
#5763=AXIS2_PLACEMENT_3D('',#8844,#7271,#7272);
#5764=AXIS2_PLACEMENT_3D('',#8845,#7273,#7274);
#5765=AXIS2_PLACEMENT_3D('',#8847,#7275,#7276);
#5766=AXIS2_PLACEMENT_3D('',#8849,#7278,#7279);
#5767=AXIS2_PLACEMENT_3D('',#8851,#7280,#7281);
#5768=AXIS2_PLACEMENT_3D('',#8853,#7283,#7284);
#5769=AXIS2_PLACEMENT_3D('',#8855,#7285,#7286);
#5770=AXIS2_PLACEMENT_3D('',#8856,#7287,#7288);
#5771=AXIS2_PLACEMENT_3D('',#8858,#7290,#7291);
#5772=AXIS2_PLACEMENT_3D('',#8859,#7292,#7293);
#5773=AXIS2_PLACEMENT_3D('',#8861,#7294,#7295);
#5774=AXIS2_PLACEMENT_3D('',#8863,#7296,#7297);
#5775=AXIS2_PLACEMENT_3D('',#8864,#7298,#7299);
#5776=AXIS2_PLACEMENT_3D('',#8867,#7301,#7302);
#5777=AXIS2_PLACEMENT_3D('',#8868,#7303,#7304);
#5778=AXIS2_PLACEMENT_3D('',#8870,#7305,#7306);
#5779=AXIS2_PLACEMENT_3D('',#8871,#7307,#7308);
#5780=AXIS2_PLACEMENT_3D('',#8873,#7310,#7311);
#5781=AXIS2_PLACEMENT_3D('',#8874,#7312,#7313);
#5782=AXIS2_PLACEMENT_3D('',#8876,#7314,#7315);
#5783=AXIS2_PLACEMENT_3D('',#8878,#7316,#7317);
#5784=AXIS2_PLACEMENT_3D('',#8879,#7318,#7319);
#5785=AXIS2_PLACEMENT_3D('',#8882,#7321,#7322);
#5786=AXIS2_PLACEMENT_3D('',#8883,#7323,#7324);
#5787=AXIS2_PLACEMENT_3D('',#8885,#7325,#7326);
#5788=AXIS2_PLACEMENT_3D('',#8886,#7327,#7328);
#5789=AXIS2_PLACEMENT_3D('',#8888,#7329,#7330);
#5790=AXIS2_PLACEMENT_3D('',#8890,#7332,#7333);
#5791=AXIS2_PLACEMENT_3D('',#8893,#7335,#7336);
#5792=AXIS2_PLACEMENT_3D('',#8894,#7337,#7338);
#5793=AXIS2_PLACEMENT_3D('',#8896,#7339,#7340);
#5794=AXIS2_PLACEMENT_3D('',#8897,#7341,#7342);
#5795=AXIS2_PLACEMENT_3D('',#8899,#7344,#7345);
#5796=AXIS2_PLACEMENT_3D('',#8900,#7346,#7347);
#5797=AXIS2_PLACEMENT_3D('',#8901,#7348,#7349);
#5798=AXIS2_PLACEMENT_3D('',#8902,#7350,#7351);
#5799=AXIS2_PLACEMENT_3D('',#8903,#7352,#7353);
#5800=AXIS2_PLACEMENT_3D('',#8904,#7354,#7355);
#5801=AXIS2_PLACEMENT_3D('',#8905,#7356,#7357);
#5802=AXIS2_PLACEMENT_3D('',#8906,#7358,#7359);
#5803=AXIS2_PLACEMENT_3D('',#8907,#7360,#7361);
#5804=AXIS2_PLACEMENT_3D('',#8908,#7362,#7363);
#5805=AXIS2_PLACEMENT_3D('',#8909,#7364,#7365);
#5806=AXIS2_PLACEMENT_3D('',#8910,#7366,#7367);
#5807=AXIS2_PLACEMENT_3D('',#8911,#7368,#7369);
#5808=AXIS2_PLACEMENT_3D('',#8912,#7370,#7371);
#5809=AXIS2_PLACEMENT_3D('',#8913,#7372,#7373);
#5810=AXIS2_PLACEMENT_3D('',#8914,#7374,#7375);
#5811=AXIS2_PLACEMENT_3D('',#8915,#7376,#7377);
#5812=AXIS2_PLACEMENT_3D('',#8916,#7378,#7379);
#5813=AXIS2_PLACEMENT_3D('',#8917,#7380,#7381);
#5814=AXIS2_PLACEMENT_3D('',#8918,#7382,#7383);
#5815=AXIS2_PLACEMENT_3D('',#8919,#7384,#7385);
#5816=AXIS2_PLACEMENT_3D('',#8920,#7386,#7387);
#5817=DIRECTION('axis',(0.,0.,1.));
#5818=DIRECTION('refdir',(1.,0.,0.));
#5819=DIRECTION('axis',(0.,0.,1.));
#5820=DIRECTION('refdir',(1.,0.,0.));
#5821=DIRECTION('center_axis',(-1.,1.34377255958835E-12,4.29697613365962E-25));
#5822=DIRECTION('ref_axis',(-1.34377255958835E-12,-1.,8.56382801334526E-17));
#5823=DIRECTION('',(-4.23473790744943E-21,-2.13480776911686E-15,1.));
#5824=DIRECTION('center_axis',(-1.,1.34421664202194E-12,4.29697613365962E-25));
#5825=DIRECTION('ref_axis',(-1.34421664202194E-12,-1.,8.56382801334526E-17));
#5826=DIRECTION('',(1.34377255958835E-12,1.,-8.56382801334526E-17));
#5827=DIRECTION('center_axis',(-1.,1.34377255958835E-12,4.44095986543338E-16));
#5828=DIRECTION('ref_axis',(4.44095986553001E-16,7.19106563773386E-15,1.));
#5829=DIRECTION('',(-4.77967767461644E-22,-8.56382801334526E-17,-1.));
#5830=DIRECTION('center_axis',(-1.,1.34332846360224E-12,4.2969924039158E-25));
#5831=DIRECTION('ref_axis',(1.34332846360224E-12,1.,-3.63835195893395E-15));
#5832=DIRECTION('',(-1.34377255958835E-12,-1.,8.56382801334526E-17));
#5833=DIRECTION('center_axis',(-1.,1.34377255958835E-12,6.77669327569707E-21));
#5834=DIRECTION('ref_axis',(-6.77670293885375E-21,-7.19106563773446E-15,
-1.));
#5835=DIRECTION('',(4.29812688450512E-25,8.56382801334526E-17,1.));
#5836=DIRECTION('center_axis',(1.,-1.34377255958835E-12,-4.29697613365962E-25));
#5837=DIRECTION('ref_axis',(4.34586730890502E-25,3.63835195893394E-15,1.));
#5838=DIRECTION('center_axis',(-1.,1.34377255958835E-12,4.29697613365962E-25));
#5839=DIRECTION('ref_axis',(-4.29812691736856E-25,-8.56382801334526E-17,
-1.));
#5840=DIRECTION('',(9.69851673070364E-22,-4.22618326275775E-16,1.));
#5841=DIRECTION('center_axis',(-1.,1.34377255281209E-12,4.29697613365962E-25));
#5842=DIRECTION('ref_axis',(-1.34377255281209E-12,-1.,8.56382801334526E-17));
#5843=DIRECTION('center_axis',(1.,-1.34377255958835E-12,-4.29697613365962E-25));
#5844=DIRECTION('ref_axis',(1.34377255958835E-12,1.,-7.19106563773443E-15));
#5845=DIRECTION('center_axis',(0.,-1.,8.57182693503055E-17));
#5846=DIRECTION('ref_axis',(0.,-8.57182693503055E-17,-1.));
#5847=DIRECTION('',(0.,-8.57182693503055E-17,-1.));
#5848=DIRECTION('',(1.,0.,0.));
#5849=DIRECTION('',(1.,0.,0.));
#5850=DIRECTION('center_axis',(0.,0.,1.));
#5851=DIRECTION('ref_axis',(1.,0.,0.));
#5852=DIRECTION('',(1.,0.,0.));
#5853=DIRECTION('',(0.,-1.,0.));
#5854=DIRECTION('',(-1.,1.34381394900629E-12,0.));
#5855=DIRECTION('center_axis',(0.,-1.,6.42887020127291E-17));
#5856=DIRECTION('ref_axis',(0.,-6.42887020127291E-17,-1.));
#5857=DIRECTION('',(1.,0.,0.));
#5858=DIRECTION('',(0.,-6.42887020127291E-17,-1.));
#5859=DIRECTION('',(-1.,1.34381394900629E-12,0.));
#5860=DIRECTION('center_axis',(0.,-1.,6.42887020127291E-17));
#5861=DIRECTION('ref_axis',(0.,-6.42887020127291E-17,-1.));
#5862=DIRECTION('center_axis',(0.,-1.,6.42887020127291E-17));
#5863=DIRECTION('ref_axis',(0.,-6.42887020127291E-17,-1.));
#5864=DIRECTION('center_axis',(0.,0.,1.));
#5865=DIRECTION('ref_axis',(1.,0.,0.));
#5866=DIRECTION('',(1.,0.,0.));
#5867=DIRECTION('',(0.,-1.,0.));
#5868=DIRECTION('',(-1.,1.34381394900629E-12,0.));
#5869=DIRECTION('center_axis',(1.,0.,0.));
#5870=DIRECTION('ref_axis',(0.,0.,-1.));
#5871=DIRECTION('center_axis',(-1.,0.,0.));
#5872=DIRECTION('ref_axis',(0.,0.,1.));
#5873=DIRECTION('',(1.,0.,0.));
#5874=DIRECTION('center_axis',(-1.,0.,0.));
#5875=DIRECTION('ref_axis',(0.,0.,1.));
#5876=DIRECTION('center_axis',(0.,-1.,8.57182693503055E-17));
#5877=DIRECTION('ref_axis',(0.,-8.57182693503055E-17,-1.));
#5878=DIRECTION('',(1.,0.,0.));
#5879=DIRECTION('',(0.,-8.57182693503055E-17,-1.));
#5880=DIRECTION('',(-1.,1.34381394900629E-12,0.));
#5881=DIRECTION('center_axis',(1.,0.,0.));
#5882=DIRECTION('ref_axis',(0.,0.,-1.));
#5883=DIRECTION('center_axis',(-1.,0.,0.));
#5884=DIRECTION('ref_axis',(0.,0.,1.));
#5885=DIRECTION('',(1.,0.,0.));
#5886=DIRECTION('center_axis',(-1.,0.,0.));
#5887=DIRECTION('ref_axis',(0.,0.,1.));
#5888=DIRECTION('center_axis',(-1.,0.,0.));
#5889=DIRECTION('ref_axis',(0.,-1.,0.));
#5890=DIRECTION('',(0.,-8.57182693503055E-17,-1.));
#5891=DIRECTION('center_axis',(-1.,0.,0.));
#5892=DIRECTION('ref_axis',(0.,0.,1.));
#5893=DIRECTION('center_axis',(-1.,0.,0.));
#5894=DIRECTION('ref_axis',(0.,0.,1.));
#5895=DIRECTION('center_axis',(-1.,0.,0.));
#5896=DIRECTION('ref_axis',(0.,0.,1.));
#5897=DIRECTION('center_axis',(-1.,0.,0.));
#5898=DIRECTION('ref_axis',(0.,0.,1.));
#5899=DIRECTION('center_axis',(-1.,0.,0.));
#5900=DIRECTION('ref_axis',(0.,0.,1.));
#5901=DIRECTION('center_axis',(-1.,0.,0.));
#5902=DIRECTION('ref_axis',(0.,0.,1.));
#5903=DIRECTION('center_axis',(-1.,0.,0.));
#5904=DIRECTION('ref_axis',(0.,0.,1.));
#5905=DIRECTION('center_axis',(-1.,0.,0.));
#5906=DIRECTION('ref_axis',(0.,0.,1.));
#5907=DIRECTION('center_axis',(-1.,0.,0.));
#5908=DIRECTION('ref_axis',(0.,-1.,0.));
#5909=DIRECTION('center_axis',(-1.,0.,0.));
#5910=DIRECTION('ref_axis',(0.,-1.,0.));
#5911=DIRECTION('center_axis',(1.,0.,0.));
#5912=DIRECTION('ref_axis',(0.,0.,-1.));
#5913=DIRECTION('center_axis',(-1.,0.,0.));
#5914=DIRECTION('ref_axis',(0.,0.,1.));
#5915=DIRECTION('center_axis',(1.,0.,0.));
#5916=DIRECTION('ref_axis',(0.,0.,-1.));
#5917=DIRECTION('center_axis',(-1.,0.,0.));
#5918=DIRECTION('ref_axis',(0.,0.,1.));
#5919=DIRECTION('center_axis',(0.,-1.,8.57182693503055E-17));
#5920=DIRECTION('ref_axis',(1.,0.,0.));
#5921=DIRECTION('',(-1.,1.34381394900629E-12,0.));
#5922=DIRECTION('center_axis',(0.,-1.,8.57182693503055E-17));
#5923=DIRECTION('ref_axis',(0.,-8.57182693503055E-17,-1.));
#5924=DIRECTION('center_axis',(0.,-1.,8.57182693503055E-17));
#5925=DIRECTION('ref_axis',(0.,-8.57182693503055E-17,-1.));
#5926=DIRECTION('',(1.,0.,0.));
#5927=DIRECTION('',(1.,0.,0.));
#5928=DIRECTION('center_axis',(0.,-1.,8.57182693503055E-17));
#5929=DIRECTION('ref_axis',(0.,-8.57182693503055E-17,-1.));
#5930=DIRECTION('',(-1.,1.34381394900629E-12,0.));
#5931=DIRECTION('center_axis',(0.,-1.,8.57182693503055E-17));
#5932=DIRECTION('ref_axis',(0.,-8.57182693503055E-17,-1.));
#5933=DIRECTION('',(0.,-1.,8.57182693503055E-17));
#5934=DIRECTION('center_axis',(0.,-1.,8.57182693503055E-17));
#5935=DIRECTION('ref_axis',(0.,-8.57182693503055E-17,-1.));
#5936=DIRECTION('',(0.,-1.,8.57182693503055E-17));
#5937=DIRECTION('center_axis',(-1.,0.,0.));
#5938=DIRECTION('ref_axis',(0.,0.,1.));
#5939=DIRECTION('',(-1.,1.34381394900629E-12,0.));
#5940=DIRECTION('center_axis',(1.,0.,0.));
#5941=DIRECTION('ref_axis',(0.,0.,-1.));
#5942=DIRECTION('center_axis',(1.,0.,0.));
#5943=DIRECTION('ref_axis',(0.,0.,-1.));
#5944=DIRECTION('',(-1.,1.34381394900629E-12,0.));
#5945=DIRECTION('center_axis',(-1.,0.,0.));
#5946=DIRECTION('ref_axis',(0.,0.,1.));
#5947=DIRECTION('axis',(0.,0.,1.));
#5948=DIRECTION('refdir',(1.,0.,0.));
#5949=DIRECTION('center_axis',(-3.49459686471004E-16,-3.44690246421401E-16,
-1.));
#5950=DIRECTION('ref_axis',(-1.34368925898019E-12,-1.,3.44690246421871E-16));
#5951=DIRECTION('',(-3.65204942310907E-16,1.,-3.446902464214E-16));
#5952=DIRECTION('',(-1.,1.34368543743058E-12,3.49459686470541E-16));
#5953=DIRECTION('',(0.,-1.,3.44690246421401E-16));
#5954=DIRECTION('',(1.,0.,-3.49459686471004E-16));
#5955=DIRECTION('center_axis',(3.49459686467822E-16,-2.0237855394456E-15,
1.));
#5956=DIRECTION('ref_axis',(1.34605772573104E-12,1.,2.02378553944513E-15));
#5957=DIRECTION('',(3.65204942310907E-16,-1.,-2.0237855394456E-15));
#5958=DIRECTION('',(-1.,0.,3.49459686467822E-16));
#5959=DIRECTION('',(0.,1.,2.0237855394456E-15));
#5960=DIRECTION('',(-1.,1.34368543743058E-12,3.49459686470541E-16));
#5961=DIRECTION('center_axis',(-1.34368543743058E-12,-1.,-2.02378553944513E-15));
#5962=DIRECTION('ref_axis',(-8.8817159728603E-16,-2.02378553944394E-15,
1.));
#5963=DIRECTION('',(-7.39096481182707E-31,2.02378553944513E-15,-1.));
#5964=DIRECTION('',(0.,-2.02378553944513E-15,1.));
#5965=DIRECTION('center_axis',(0.,1.,0.));
#5966=DIRECTION('ref_axis',(0.,0.,1.));
#5967=DIRECTION('',(0.,0.,-1.));
#5968=DIRECTION('',(1.,0.,0.));
#5969=DIRECTION('',(0.,0.,-1.));
#5970=DIRECTION('',(-1.,0.,0.));
#5971=DIRECTION('',(0.,0.,-1.));
#5972=DIRECTION('',(1.,0.,0.));
#5973=DIRECTION('',(0.,0.,-1.));
#5974=DIRECTION('center_axis',(0.,1.,0.));
#5975=DIRECTION('ref_axis',(0.,0.,1.));
#5976=DIRECTION('',(0.,0.,-1.));
#5977=DIRECTION('',(1.,0.,0.));
#5978=DIRECTION('',(0.,0.,-1.));
#5979=DIRECTION('',(-1.,0.,0.));
#5980=DIRECTION('',(0.,0.,-1.));
#5981=DIRECTION('',(1.,0.,0.));
#5982=DIRECTION('',(0.,0.,-1.));
#5983=DIRECTION('center_axis',(-1.,-3.65204942310907E-16,0.));
#5984=DIRECTION('ref_axis',(3.65204942310907E-16,-1.,0.));
#5985=DIRECTION('',(-3.65204942310907E-16,1.,0.));
#5986=DIRECTION('',(0.,0.,-1.));
#5987=DIRECTION('',(-3.65204942310907E-16,1.,0.));
#5988=DIRECTION('center_axis',(1.34368925898019E-12,1.,-5.08164181815587E-15));
#5989=DIRECTION('ref_axis',(3.55268652758613E-15,-5.08164181816064E-15,
-1.));
#5990=DIRECTION('',(0.,5.08164181815587E-15,1.));
#5991=DIRECTION('',(-1.,1.34368925898019E-12,-2.5823130969E-16));
#5992=DIRECTION('',(-3.55268652758613E-15,5.08164181816065E-15,1.));
#5993=DIRECTION('',(1.,0.,0.));
#5994=DIRECTION('center_axis',(2.5823130969E-16,-3.46795905806759E-28,-1.));
#5995=DIRECTION('ref_axis',(1.,-1.3429252284855E-12,2.5823130969E-16));
#5996=DIRECTION('',(-1.34296614234377E-12,-1.,0.));
#5997=DIRECTION('',(-1.,1.3429252284855E-12,-2.5823130969E-16));
#5998=DIRECTION('',(-1.34296614234377E-12,-1.,0.));
#5999=DIRECTION('center_axis',(1.3429252284855E-12,1.,9.98628687409672E-23));
#6000=DIRECTION('ref_axis',(-1.,1.3429252284855E-12,1.26981758441774E-15));
#6001=DIRECTION('',(1.,-1.34216120476708E-12,2.5823130969E-16));
#6002=DIRECTION('',(-1.26981758441774E-15,9.98645738638139E-23,-1.));
#6003=DIRECTION('',(1.26981758440819E-15,-7.1054274574656E-15,1.));
#6004=DIRECTION('center_axis',(0.,0.,1.));
#6005=DIRECTION('ref_axis',(1.,0.,0.));
#6006=DIRECTION('',(1.82602471155453E-16,-1.,0.));
#6007=DIRECTION('',(1.,0.,0.));
#6008=DIRECTION('',(0.,-1.,0.));
#6009=DIRECTION('',(1.,0.,0.));
#6010=DIRECTION('',(0.,-1.,0.));
#6011=DIRECTION('',(1.,0.,0.));
#6012=DIRECTION('',(0.,-1.,0.));
#6013=DIRECTION('',(1.,5.78241158658936E-16,0.));
#6014=DIRECTION('',(0.,-1.,0.));
#6015=DIRECTION('',(1.,0.,0.));
#6016=DIRECTION('',(1.,0.,0.));
#6017=DIRECTION('',(0.,-1.,0.));
#6018=DIRECTION('',(1.,0.,0.));
#6019=DIRECTION('',(0.,-1.,0.));
#6020=DIRECTION('',(1.,0.,0.));
#6021=DIRECTION('',(1.7347234759768E-16,-1.,0.));
#6022=DIRECTION('',(1.,2.89120579329468E-16,0.));
#6023=DIRECTION('',(0.,-1.,0.));
#6024=DIRECTION('',(1.,0.,0.));
#6025=DIRECTION('',(0.,-1.,0.));
#6026=DIRECTION('',(1.,0.,0.));
#6027=DIRECTION('',(1.7347234759768E-16,-1.,0.));
#6028=DIRECTION('',(0.,-1.,0.));
#6029=DIRECTION('',(1.,0.,0.));
#6030=DIRECTION('',(0.,-1.,0.));
#6031=DIRECTION('',(1.,0.,0.));
#6032=DIRECTION('',(-1.,0.,0.));
#6033=DIRECTION('',(0.,1.,0.));
#6034=DIRECTION('',(-1.,0.,0.));
#6035=DIRECTION('',(-1.7347234759768E-16,1.,0.));
#6036=DIRECTION('',(1.,0.,0.));
#6037=DIRECTION('',(0.,-1.,0.));
#6038=DIRECTION('',(1.,0.,0.));
#6039=DIRECTION('',(0.,-1.,0.));
#6040=DIRECTION('center_axis',(1.,0.,0.));
#6041=DIRECTION('ref_axis',(0.,0.,-1.));
#6042=DIRECTION('center_axis',(1.,0.,0.));
#6043=DIRECTION('ref_axis',(0.,0.,-1.));
#6044=DIRECTION('',(0.,-1.,0.));
#6045=DIRECTION('',(0.,0.,-1.));
#6046=DIRECTION('center_axis',(1.,0.,0.));
#6047=DIRECTION('ref_axis',(0.,0.,-1.));
#6048=DIRECTION('',(0.,-1.,0.));
#6049=DIRECTION('center_axis',(1.,0.,0.));
#6050=DIRECTION('ref_axis',(0.,0.,-1.));
#6051=DIRECTION('',(0.,0.,-1.));
#6052=DIRECTION('center_axis',(1.,0.,0.));
#6053=DIRECTION('ref_axis',(0.,0.,-1.));
#6054=DIRECTION('center_axis',(1.,0.,0.));
#6055=DIRECTION('ref_axis',(0.,0.,-1.));
#6056=DIRECTION('',(0.,-1.,0.));
#6057=DIRECTION('',(0.,0.,-1.));
#6058=DIRECTION('center_axis',(1.,0.,0.));
#6059=DIRECTION('ref_axis',(0.,0.,-1.));
#6060=DIRECTION('',(0.,-1.,0.));
#6061=DIRECTION('center_axis',(1.,0.,0.));
#6062=DIRECTION('ref_axis',(0.,0.,-1.));
#6063=DIRECTION('',(0.,0.,-1.));
#6064=DIRECTION('center_axis',(1.,1.7347234759768E-16,0.));
#6065=DIRECTION('ref_axis',(-1.7347234759768E-16,1.,0.));
#6066=DIRECTION('center_axis',(1.,1.7347234759768E-16,0.));
#6067=DIRECTION('ref_axis',(-1.7347234759768E-16,1.,0.));
#6068=DIRECTION('',(0.,0.,-1.));
#6069=DIRECTION('',(1.7347234759768E-16,-1.,0.));
#6070=DIRECTION('center_axis',(-1.,-1.7347234759768E-16,0.));
#6071=DIRECTION('ref_axis',(1.7347234759768E-16,-1.,0.));
#6072=DIRECTION('center_axis',(-1.,-1.7347234759768E-16,0.));
#6073=DIRECTION('ref_axis',(1.7347234759768E-16,-1.,0.));
#6074=DIRECTION('',(0.,0.,-1.));
#6075=DIRECTION('',(-1.7347234759768E-16,1.,0.));
#6076=DIRECTION('center_axis',(0.,-1.,0.));
#6077=DIRECTION('ref_axis',(0.,0.,-1.));
#6078=DIRECTION('',(-1.,0.,0.));
#6079=DIRECTION('',(0.,0.,-1.));
#6080=DIRECTION('',(-1.,0.,0.));
#6081=DIRECTION('center_axis',(1.,1.7347234759768E-16,0.));
#6082=DIRECTION('ref_axis',(-1.7347234759768E-16,1.,0.));
#6083=DIRECTION('',(0.,0.,-1.));
#6084=DIRECTION('center_axis',(1.,1.7347234759768E-16,0.));
#6085=DIRECTION('ref_axis',(-1.7347234759768E-16,1.,0.));
#6086=DIRECTION('',(1.7347234759768E-16,-1.,0.));
#6087=DIRECTION('center_axis',(1.,0.,0.));
#6088=DIRECTION('ref_axis',(0.,0.,-1.));
#6089=DIRECTION('center_axis',(1.,0.,0.));
#6090=DIRECTION('ref_axis',(0.,0.,-1.));
#6091=DIRECTION('',(0.,-1.,0.));
#6092=DIRECTION('',(0.,0.,-1.));
#6093=DIRECTION('center_axis',(1.,0.,0.));
#6094=DIRECTION('ref_axis',(0.,0.,-1.));
#6095=DIRECTION('',(0.,-1.,0.));
#6096=DIRECTION('center_axis',(1.,0.,0.));
#6097=DIRECTION('ref_axis',(0.,0.,-1.));
#6098=DIRECTION('',(0.,0.,-1.));
#6099=DIRECTION('center_axis',(0.,0.,1.));
#6100=DIRECTION('ref_axis',(1.,0.,0.));
#6101=DIRECTION('',(0.,-1.,0.));
#6102=DIRECTION('',(-1.,0.,0.));
#6103=DIRECTION('',(1.,0.,0.));
#6104=DIRECTION('',(-1.,0.,0.));
#6105=DIRECTION('',(1.,0.,0.));
#6106=DIRECTION('',(-1.,0.,0.));
#6107=DIRECTION('',(0.,1.,0.));
#6108=DIRECTION('',(-1.,0.,0.));
#6109=DIRECTION('',(1.,0.,0.));
#6110=DIRECTION('',(-1.,0.,0.));
#6111=DIRECTION('',(0.,-1.,0.));
#6112=DIRECTION('',(1.,0.,0.));
#6113=DIRECTION('center_axis',(0.,0.,1.));
#6114=DIRECTION('ref_axis',(1.,0.,0.));
#6115=DIRECTION('',(0.,-1.,0.));
#6116=DIRECTION('',(0.,-1.,0.));
#6117=DIRECTION('center_axis',(0.,0.,1.));
#6118=DIRECTION('ref_axis',(1.,0.,0.));
#6119=DIRECTION('',(1.82602471155453E-16,-1.,0.));
#6120=DIRECTION('',(1.,0.,0.));
#6121=DIRECTION('',(0.,-1.,0.));
#6122=DIRECTION('',(-1.,0.,0.));
#6123=DIRECTION('',(0.,-1.,0.));
#6124=DIRECTION('',(-1.,0.,0.));
#6125=DIRECTION('',(-1.,0.,0.));
#6126=DIRECTION('',(0.,-1.,0.));
#6127=DIRECTION('',(-1.,0.,0.));
#6128=DIRECTION('',(0.,-1.,0.));
#6129=DIRECTION('',(1.7347234759768E-16,1.,0.));
#6130=DIRECTION('',(1.,-2.89120579329468E-16,0.));
#6131=DIRECTION('',(0.,1.,0.));
#6132=DIRECTION('',(1.,-1.44560289664734E-16,0.));
#6133=DIRECTION('',(-1.,2.89120579329468E-16,0.));
#6134=DIRECTION('',(-1.7347234759768E-16,-1.,0.));
#6135=DIRECTION('',(-1.,2.89120579329468E-16,0.));
#6136=DIRECTION('',(0.,-1.,0.));
#6137=DIRECTION('',(-1.,0.,0.));
#6138=DIRECTION('',(0.,-1.,0.));
#6139=DIRECTION('',(-1.,0.,0.));
#6140=DIRECTION('',(0.,-1.,0.));
#6141=DIRECTION('',(0.,-1.,0.));
#6142=DIRECTION('',(-1.,0.,0.));
#6143=DIRECTION('',(0.,-1.,0.));
#6144=DIRECTION('',(-1.,0.,0.));
#6145=DIRECTION('',(-1.7347234759768E-16,-1.,0.));
#6146=DIRECTION('',(-1.,0.,0.));
#6147=DIRECTION('',(0.,-1.,0.));
#6148=DIRECTION('',(-1.,0.,0.));
#6149=DIRECTION('',(0.,-1.,0.));
#6150=DIRECTION('',(-1.,5.78241158658936E-16,0.));
#6151=DIRECTION('',(-1.73472347597681E-16,-1.,0.));
#6152=DIRECTION('',(-1.,0.,0.));
#6153=DIRECTION('center_axis',(1.,0.,0.));
#6154=DIRECTION('ref_axis',(0.,0.,-1.));
#6155=DIRECTION('center_axis',(1.,0.,0.));
#6156=DIRECTION('ref_axis',(0.,0.,-1.));
#6157=DIRECTION('',(0.,1.,0.));
#6158=DIRECTION('',(0.,0.,1.));
#6159=DIRECTION('center_axis',(1.,0.,0.));
#6160=DIRECTION('ref_axis',(0.,0.,-1.));
#6161=DIRECTION('',(0.,1.,0.));
#6162=DIRECTION('center_axis',(1.,0.,0.));
#6163=DIRECTION('ref_axis',(0.,0.,-1.));
#6164=DIRECTION('',(0.,0.,1.));
#6165=DIRECTION('center_axis',(1.,0.,0.));
#6166=DIRECTION('ref_axis',(0.,0.,-1.));
#6167=DIRECTION('',(0.,1.,0.));
#6168=DIRECTION('center_axis',(1.,0.,0.));
#6169=DIRECTION('ref_axis',(0.,0.,-1.));
#6170=DIRECTION('',(0.,0.,1.));
#6171=DIRECTION('center_axis',(0.,-1.,0.));
#6172=DIRECTION('ref_axis',(0.,0.,-1.));
#6173=DIRECTION('',(0.,0.,1.));
#6174=DIRECTION('',(1.,0.,0.));
#6175=DIRECTION('',(0.,0.,1.));
#6176=DIRECTION('',(1.,0.,0.));
#6177=DIRECTION('center_axis',(0.,-1.,0.));
#6178=DIRECTION('ref_axis',(0.,0.,-1.));
#6179=DIRECTION('',(0.,0.,1.));
#6180=DIRECTION('',(1.,0.,0.));
#6181=DIRECTION('',(0.,0.,1.));
#6182=DIRECTION('',(1.,0.,0.));
#6183=DIRECTION('center_axis',(0.,-1.,0.));
#6184=DIRECTION('ref_axis',(0.,0.,-1.));
#6185=DIRECTION('',(0.,0.,1.));
#6186=DIRECTION('',(1.,0.,0.));
#6187=DIRECTION('',(0.,0.,1.));
#6188=DIRECTION('',(1.,0.,0.));
#6189=DIRECTION('center_axis',(1.,0.,0.));
#6190=DIRECTION('ref_axis',(0.,0.,-1.));
#6191=DIRECTION('center_axis',(1.,0.,0.));
#6192=DIRECTION('ref_axis',(0.,0.,-1.));
#6193=DIRECTION('',(0.,1.,0.));
#6194=DIRECTION('',(0.,0.,1.));
#6195=DIRECTION('center_axis',(1.,0.,0.));
#6196=DIRECTION('ref_axis',(0.,0.,-1.));
#6197=DIRECTION('',(0.,1.,0.));
#6198=DIRECTION('center_axis',(1.,0.,0.));
#6199=DIRECTION('ref_axis',(0.,0.,-1.));
#6200=DIRECTION('',(0.,0.,1.));
#6201=DIRECTION('center_axis',(0.,-1.,0.));
#6202=DIRECTION('ref_axis',(0.,0.,-1.));
#6203=DIRECTION('',(0.,0.,1.));
#6204=DIRECTION('',(1.,0.,0.));
#6205=DIRECTION('',(0.,0.,1.));
#6206=DIRECTION('',(1.,0.,0.));
#6207=DIRECTION('center_axis',(0.,-1.,0.));
#6208=DIRECTION('ref_axis',(0.,0.,-1.));
#6209=DIRECTION('',(1.,0.,0.));
#6210=DIRECTION('',(1.,0.,0.));
#6211=DIRECTION('center_axis',(-2.89120579329468E-16,-1.,0.));
#6212=DIRECTION('ref_axis',(1.,-2.89120579329468E-16,0.));
#6213=DIRECTION('',(1.,0.,0.));
#6214=DIRECTION('',(0.,0.,1.));
#6215=DIRECTION('',(1.,-2.89120579329468E-16,0.));
#6216=DIRECTION('center_axis',(0.,-1.,0.));
#6217=DIRECTION('ref_axis',(0.,0.,-1.));
#6218=DIRECTION('',(1.,0.,0.));
#6219=DIRECTION('',(1.,0.,0.));
#6220=DIRECTION('center_axis',(0.,0.,-1.));
#6221=DIRECTION('ref_axis',(1.,0.,0.));
#6222=DIRECTION('',(0.,-1.,0.));
#6223=DIRECTION('',(1.,0.,0.));
#6224=DIRECTION('',(0.,1.,0.));
#6225=DIRECTION('',(0.,1.,0.));
#6226=DIRECTION('',(1.,0.,0.));
#6227=DIRECTION('',(0.,1.,0.));
#6228=DIRECTION('',(1.73472347597681E-16,1.,0.));
#6229=DIRECTION('',(1.,0.,0.));
#6230=DIRECTION('',(1.7347234759768E-16,1.,0.));
#6231=DIRECTION('',(0.,1.,0.));
#6232=DIRECTION('',(1.,0.,0.));
#6233=DIRECTION('',(0.,1.,0.));
#6234=DIRECTION('',(0.,1.,0.));
#6235=DIRECTION('',(1.,0.,0.));
#6236=DIRECTION('',(0.,-1.,0.));
#6237=DIRECTION('',(1.,0.,0.));
#6238=DIRECTION('center_axis',(0.,0.,1.));
#6239=DIRECTION('ref_axis',(1.,0.,0.));
#6240=DIRECTION('',(0.,-1.,0.));
#6241=DIRECTION('',(1.,0.,0.));
#6242=DIRECTION('',(0.,-1.,0.));
#6243=DIRECTION('center_axis',(1.,1.82602471155453E-16,0.));
#6244=DIRECTION('ref_axis',(-1.82602471155453E-16,1.,0.));
#6245=DIRECTION('',(3.16764793484742E-32,-1.7347234759768E-16,-1.));
#6246=DIRECTION('',(-1.82602471155453E-16,1.,0.));
#6247=DIRECTION('',(0.,0.,-1.));
#6248=DIRECTION('',(-1.82602471155453E-16,1.,0.));
#6249=DIRECTION('center_axis',(1.,0.,0.));
#6250=DIRECTION('ref_axis',(0.,0.,-1.));
#6251=DIRECTION('center_axis',(-1.,0.,0.));
#6252=DIRECTION('ref_axis',(0.,0.,1.));
#6253=DIRECTION('',(0.,-1.,0.));
#6254=DIRECTION('',(0.,-1.,0.));
#6255=DIRECTION('',(0.,1.7347234759768E-16,1.));
#6256=DIRECTION('',(0.,-1.,0.));
#6257=DIRECTION('center_axis',(1.,0.,0.));
#6258=DIRECTION('ref_axis',(0.,0.,-1.));
#6259=DIRECTION('',(0.,0.,1.));
#6260=DIRECTION('',(0.,-1.,0.));
#6261=DIRECTION('center_axis',(1.,0.,0.));
#6262=DIRECTION('ref_axis',(0.,0.,-1.));
#6263=DIRECTION('',(0.,0.,-1.));
#6264=DIRECTION('center_axis',(0.,1.,0.));
#6265=DIRECTION('ref_axis',(0.,0.,1.));
#6266=DIRECTION('',(0.,0.,-1.));
#6267=DIRECTION('center_axis',(0.,-1.,0.));
#6268=DIRECTION('ref_axis',(0.,0.,-1.));
#6269=DIRECTION('center_axis',(0.,-1.,0.));
#6270=DIRECTION('ref_axis',(0.,0.,-1.));
#6271=DIRECTION('center_axis',(0.,-1.,0.));
#6272=DIRECTION('ref_axis',(0.,0.,-1.));
#6273=DIRECTION('center_axis',(0.,-1.,0.));
#6274=DIRECTION('ref_axis',(0.,0.,-1.));
#6275=DIRECTION('center_axis',(0.,-1.,0.));
#6276=DIRECTION('ref_axis',(0.,0.,-1.));
#6277=DIRECTION('center_axis',(1.,0.,0.));
#6278=DIRECTION('ref_axis',(0.,0.,-1.));
#6279=DIRECTION('',(0.,-1.,0.));
#6280=DIRECTION('center_axis',(1.,0.,0.));
#6281=DIRECTION('ref_axis',(0.,0.,-1.));
#6282=DIRECTION('center_axis',(1.,0.,0.));
#6283=DIRECTION('ref_axis',(0.,0.,-1.));
#6284=DIRECTION('',(0.,-1.,0.));
#6285=DIRECTION('',(0.,0.,1.));
#6286=DIRECTION('center_axis',(1.,0.,0.));
#6287=DIRECTION('ref_axis',(0.,0.,-1.));
#6288=DIRECTION('center_axis',(0.,1.,0.));
#6289=DIRECTION('ref_axis',(0.,0.,1.));
#6290=DIRECTION('center_axis',(0.,1.,0.));
#6291=DIRECTION('ref_axis',(0.,0.,1.));
#6292=DIRECTION('center_axis',(0.,1.,0.));
#6293=DIRECTION('ref_axis',(0.,0.,1.));
#6294=DIRECTION('center_axis',(0.,1.,0.));
#6295=DIRECTION('ref_axis',(0.,0.,1.));
#6296=DIRECTION('center_axis',(0.,1.,0.));
#6297=DIRECTION('ref_axis',(0.,0.,1.));
#6298=DIRECTION('center_axis',(0.,1.,0.));
#6299=DIRECTION('ref_axis',(0.,0.,1.));
#6300=DIRECTION('center_axis',(0.,0.,-1.));
#6301=DIRECTION('ref_axis',(-1.,0.,0.));
#6302=DIRECTION('',(-1.,0.,0.));
#6303=DIRECTION('center_axis',(0.,0.,-1.));
#6304=DIRECTION('ref_axis',(-1.,0.,0.));
#6305=DIRECTION('',(-1.,0.,0.));
#6306=DIRECTION('center_axis',(0.,-1.,1.7347234759768E-16));
#6307=DIRECTION('ref_axis',(0.,-1.7347234759768E-16,-1.));
#6308=DIRECTION('center_axis',(0.,-1.,0.));
#6309=DIRECTION('ref_axis',(0.,0.,-1.));
#6310=DIRECTION('',(0.,-1.,0.));
#6311=DIRECTION('center_axis',(0.,-1.,0.));
#6312=DIRECTION('ref_axis',(0.,0.,-1.));
#6313=DIRECTION('',(0.,-1.,0.));
#6314=DIRECTION('center_axis',(0.,-1.,0.));
#6315=DIRECTION('ref_axis',(0.,0.,-1.));
#6316=DIRECTION('',(0.,-1.,0.));
#6317=DIRECTION('center_axis',(0.,-1.,0.));
#6318=DIRECTION('ref_axis',(0.,0.,-1.));
#6319=DIRECTION('',(0.,-1.,0.));
#6320=DIRECTION('center_axis',(0.,-1.,0.));
#6321=DIRECTION('ref_axis',(0.,0.,-1.));
#6322=DIRECTION('',(0.,-1.,0.));
#6323=DIRECTION('center_axis',(0.,-1.,0.));
#6324=DIRECTION('ref_axis',(0.,0.,-1.));
#6325=DIRECTION('',(1.,0.,0.));
#6326=DIRECTION('',(1.,0.,0.));
#6327=DIRECTION('center_axis',(1.,-1.7347234759768E-16,0.));
#6328=DIRECTION('ref_axis',(1.7347234759768E-16,1.,0.));
#6329=DIRECTION('center_axis',(1.,-1.7347234759768E-16,0.));
#6330=DIRECTION('ref_axis',(1.7347234759768E-16,1.,0.));
#6331=DIRECTION('',(1.7347234759768E-16,1.,0.));
#6332=DIRECTION('center_axis',(1.,0.,0.));
#6333=DIRECTION('ref_axis',(0.,0.,-1.));
#6334=DIRECTION('center_axis',(1.,0.,0.));
#6335=DIRECTION('ref_axis',(0.,0.,-1.));
#6336=DIRECTION('center_axis',(1.,0.,0.));
#6337=DIRECTION('ref_axis',(0.,0.,-1.));
#6338=DIRECTION('center_axis',(1.,0.,0.));
#6339=DIRECTION('ref_axis',(0.,0.,-1.));
#6340=DIRECTION('center_axis',(1.,-1.7347234759768E-16,0.));
#6341=DIRECTION('ref_axis',(1.7347234759768E-16,1.,0.));
#6342=DIRECTION('center_axis',(1.,-1.7347234759768E-16,0.));
#6343=DIRECTION('ref_axis',(1.7347234759768E-16,1.,0.));
#6344=DIRECTION('center_axis',(1.,0.,0.));
#6345=DIRECTION('ref_axis',(0.,0.,-1.));
#6346=DIRECTION('center_axis',(1.,0.,0.));
#6347=DIRECTION('ref_axis',(0.,0.,-1.));
#6348=DIRECTION('center_axis',(-1.,1.7347234759768E-16,0.));
#6349=DIRECTION('ref_axis',(-1.7347234759768E-16,-1.,0.));
#6350=DIRECTION('center_axis',(-1.,1.7347234759768E-16,0.));
#6351=DIRECTION('ref_axis',(-1.7347234759768E-16,-1.,0.));
#6352=DIRECTION('',(0.,0.,1.));
#6353=DIRECTION('',(-1.7347234759768E-16,-1.,0.));
#6354=DIRECTION('center_axis',(1.44560289664734E-16,1.,0.));
#6355=DIRECTION('ref_axis',(-1.,1.44560289664734E-16,0.));
#6356=DIRECTION('',(1.,0.,0.));
#6357=DIRECTION('',(0.,0.,1.));
#6358=DIRECTION('',(-1.,1.44560289664734E-16,0.));
#6359=DIRECTION('center_axis',(-1.,0.,0.));
#6360=DIRECTION('ref_axis',(0.,0.,1.));
#6361=DIRECTION('center_axis',(-1.,0.,0.));
#6362=DIRECTION('ref_axis',(0.,0.,1.));
#6363=DIRECTION('',(0.,-1.,0.));
#6364=DIRECTION('center_axis',(1.,0.,0.));
#6365=DIRECTION('ref_axis',(0.,0.,-1.));
#6366=DIRECTION('center_axis',(1.,0.,0.));
#6367=DIRECTION('ref_axis',(0.,0.,-1.));
#6368=DIRECTION('center_axis',(1.,-1.73472347597681E-16,0.));
#6369=DIRECTION('ref_axis',(1.73472347597681E-16,1.,0.));
#6370=DIRECTION('center_axis',(1.,-1.73472347597681E-16,0.));
#6371=DIRECTION('ref_axis',(1.73472347597681E-16,1.,0.));
#6372=DIRECTION('center_axis',(1.,0.,0.));
#6373=DIRECTION('ref_axis',(0.,0.,-1.));
#6374=DIRECTION('center_axis',(1.,0.,0.));
#6375=DIRECTION('ref_axis',(0.,0.,-1.));
#6376=DIRECTION('center_axis',(1.,0.,0.));
#6377=DIRECTION('ref_axis',(0.,0.,-1.));
#6378=DIRECTION('center_axis',(1.,0.,0.));
#6379=DIRECTION('ref_axis',(0.,0.,-1.));
#6380=DIRECTION('center_axis',(0.,0.,-1.));
#6381=DIRECTION('ref_axis',(1.,0.,0.));
#6382=DIRECTION('',(1.,0.,0.));
#6383=DIRECTION('',(1.,0.,0.));
#6384=DIRECTION('',(1.,0.,0.));
#6385=DIRECTION('',(1.,0.,0.));
#6386=DIRECTION('',(1.,0.,0.));
#6387=DIRECTION('center_axis',(1.,0.,0.));
#6388=DIRECTION('ref_axis',(0.,5.66553889764798E-16,1.));
#6389=DIRECTION('center_axis',(1.,0.,0.));
#6390=DIRECTION('ref_axis',(0.,0.,-1.));
#6391=DIRECTION('',(1.,0.,0.));
#6392=DIRECTION('center_axis',(1.,0.,0.));
#6393=DIRECTION('ref_axis',(0.,0.,-1.));
#6394=DIRECTION('',(1.,0.,0.));
#6395=DIRECTION('center_axis',(1.,-1.7347234759768E-16,0.));
#6396=DIRECTION('ref_axis',(1.7347234759768E-16,1.,0.));
#6397=DIRECTION('',(1.,0.,0.));
#6398=DIRECTION('center_axis',(1.,0.,0.));
#6399=DIRECTION('ref_axis',(0.,0.,-1.));
#6400=DIRECTION('',(1.,0.,0.));
#6401=DIRECTION('',(1.,0.,0.));
#6402=DIRECTION('center_axis',(1.,0.,0.));
#6403=DIRECTION('ref_axis',(0.,0.,-1.));
#6404=DIRECTION('',(1.,0.,0.));
#6405=DIRECTION('center_axis',(1.,0.,0.));
#6406=DIRECTION('ref_axis',(0.,0.,-1.));
#6407=DIRECTION('',(1.,0.,0.));
#6408=DIRECTION('center_axis',(1.,-1.7347234759768E-16,0.));
#6409=DIRECTION('ref_axis',(1.7347234759768E-16,1.,0.));
#6410=DIRECTION('',(1.,0.,0.));
#6411=DIRECTION('center_axis',(1.,0.,0.));
#6412=DIRECTION('ref_axis',(0.,0.,-1.));
#6413=DIRECTION('',(1.,0.,0.));
#6414=DIRECTION('center_axis',(-1.,1.7347234759768E-16,0.));
#6415=DIRECTION('ref_axis',(-1.7347234759768E-16,-1.,0.));
#6416=DIRECTION('',(1.,0.,0.));
#6417=DIRECTION('center_axis',(-1.,0.,0.));
#6418=DIRECTION('ref_axis',(0.,0.,1.));
#6419=DIRECTION('',(1.,0.,0.));
#6420=DIRECTION('center_axis',(1.,0.,0.));
#6421=DIRECTION('ref_axis',(0.,0.,-1.));
#6422=DIRECTION('',(1.,0.,0.));
#6423=DIRECTION('center_axis',(1.,-1.73472347597681E-16,0.));
#6424=DIRECTION('ref_axis',(1.73472347597681E-16,1.,0.));
#6425=DIRECTION('center_axis',(1.,0.,0.));
#6426=DIRECTION('ref_axis',(0.,0.,-1.));
#6427=DIRECTION('',(1.,0.,0.));
#6428=DIRECTION('center_axis',(1.,0.,0.));
#6429=DIRECTION('ref_axis',(0.,0.,-1.));
#6430=DIRECTION('',(1.,0.,0.));
#6431=DIRECTION('',(1.,0.,0.));
#6432=DIRECTION('center_axis',(1.,0.,0.));
#6433=DIRECTION('ref_axis',(0.,0.,-1.));
#6434=DIRECTION('',(1.,0.,0.));
#6435=DIRECTION('center_axis',(1.,0.,0.));
#6436=DIRECTION('ref_axis',(0.,0.,-1.));
#6437=DIRECTION('center_axis',(1.,0.,0.));
#6438=DIRECTION('ref_axis',(0.,0.,-1.));
#6439=DIRECTION('center_axis',(1.,0.,0.));
#6440=DIRECTION('ref_axis',(0.,0.,-1.));
#6441=DIRECTION('center_axis',(1.,0.,0.));
#6442=DIRECTION('ref_axis',(0.,0.,-1.));
#6443=DIRECTION('',(0.,0.,1.));
#6444=DIRECTION('center_axis',(0.,-1.,0.));
#6445=DIRECTION('ref_axis',(0.,0.,-1.));
#6446=DIRECTION('',(0.,0.,1.));
#6447=DIRECTION('center_axis',(1.,0.,0.));
#6448=DIRECTION('ref_axis',(0.,0.,-1.));
#6449=DIRECTION('center_axis',(1.,0.,0.));
#6450=DIRECTION('ref_axis',(0.,0.,-1.));
#6451=DIRECTION('center_axis',(1.,0.,0.));
#6452=DIRECTION('ref_axis',(0.,0.,-1.));
#6453=DIRECTION('center_axis',(0.,-1.,0.));
#6454=DIRECTION('ref_axis',(0.,0.,-1.));
#6455=DIRECTION('',(0.,0.,1.));
#6456=DIRECTION('',(0.,0.,1.));
#6457=DIRECTION('center_axis',(1.,0.,0.));
#6458=DIRECTION('ref_axis',(0.,0.,-1.));
#6459=DIRECTION('center_axis',(1.,0.,0.));
#6460=DIRECTION('ref_axis',(0.,0.,-1.));
#6461=DIRECTION('center_axis',(1.,0.,0.));
#6462=DIRECTION('ref_axis',(0.,0.,-1.));
#6463=DIRECTION('center_axis',(1.,0.,0.));
#6464=DIRECTION('ref_axis',(0.,0.,-1.));
#6465=DIRECTION('center_axis',(1.,0.,0.));
#6466=DIRECTION('ref_axis',(0.,0.,-1.));
#6467=DIRECTION('center_axis',(1.,0.,0.));
#6468=DIRECTION('ref_axis',(0.,0.,-1.));
#6469=DIRECTION('center_axis',(1.,-1.73472347597681E-16,0.));
#6470=DIRECTION('ref_axis',(1.73472347597681E-16,1.,0.));
#6471=DIRECTION('center_axis',(1.,-1.73472347597681E-16,0.));
#6472=DIRECTION('ref_axis',(1.73472347597681E-16,1.,0.));
#6473=DIRECTION('center_axis',(1.,-1.73472347597681E-16,0.));
#6474=DIRECTION('ref_axis',(1.73472347597681E-16,1.,0.));
#6475=DIRECTION('',(0.,0.,1.));
#6476=DIRECTION('center_axis',(0.,-1.,0.));
#6477=DIRECTION('ref_axis',(0.,0.,-1.));
#6478=DIRECTION('',(0.,0.,1.));
#6479=DIRECTION('center_axis',(1.,0.,0.));
#6480=DIRECTION('ref_axis',(0.,0.,-1.));
#6481=DIRECTION('center_axis',(1.,0.,0.));
#6482=DIRECTION('ref_axis',(0.,0.,-1.));
#6483=DIRECTION('center_axis',(1.,0.,0.));
#6484=DIRECTION('ref_axis',(0.,0.,-1.));
#6485=DIRECTION('center_axis',(-1.,0.,0.));
#6486=DIRECTION('ref_axis',(0.,0.,1.));
#6487=DIRECTION('center_axis',(-1.,0.,0.));
#6488=DIRECTION('ref_axis',(0.,0.,1.));
#6489=DIRECTION('center_axis',(-1.,0.,0.));
#6490=DIRECTION('ref_axis',(0.,0.,1.));
#6491=DIRECTION('',(0.,0.,1.));
#6492=DIRECTION('center_axis',(1.44560289664734E-16,1.,0.));
#6493=DIRECTION('ref_axis',(-1.,1.44560289664734E-16,0.));
#6494=DIRECTION('',(0.,0.,1.));
#6495=DIRECTION('center_axis',(-1.,1.7347234759768E-16,0.));
#6496=DIRECTION('ref_axis',(-1.7347234759768E-16,-1.,0.));
#6497=DIRECTION('center_axis',(-1.,1.7347234759768E-16,0.));
#6498=DIRECTION('ref_axis',(-1.7347234759768E-16,-1.,0.));
#6499=DIRECTION('center_axis',(-1.,1.7347234759768E-16,0.));
#6500=DIRECTION('ref_axis',(-1.7347234759768E-16,-1.,0.));
#6501=DIRECTION('center_axis',(1.,0.,0.));
#6502=DIRECTION('ref_axis',(0.,0.,-1.));
#6503=DIRECTION('center_axis',(1.,0.,0.));
#6504=DIRECTION('ref_axis',(0.,0.,-1.));
#6505=DIRECTION('center_axis',(1.,0.,0.));
#6506=DIRECTION('ref_axis',(0.,0.,-1.));
#6507=DIRECTION('',(0.,0.,1.));
#6508=DIRECTION('center_axis',(0.,-1.,0.));
#6509=DIRECTION('ref_axis',(0.,0.,-1.));
#6510=DIRECTION('',(0.,0.,1.));
#6511=DIRECTION('center_axis',(1.,-1.7347234759768E-16,0.));
#6512=DIRECTION('ref_axis',(1.7347234759768E-16,1.,0.));
#6513=DIRECTION('center_axis',(1.,-1.7347234759768E-16,0.));
#6514=DIRECTION('ref_axis',(1.7347234759768E-16,1.,0.));
#6515=DIRECTION('center_axis',(1.,-1.7347234759768E-16,0.));
#6516=DIRECTION('ref_axis',(1.7347234759768E-16,1.,0.));
#6517=DIRECTION('center_axis',(1.,0.,0.));
#6518=DIRECTION('ref_axis',(0.,0.,-1.));
#6519=DIRECTION('center_axis',(1.,0.,0.));
#6520=DIRECTION('ref_axis',(0.,0.,-1.));
#6521=DIRECTION('center_axis',(1.,0.,0.));
#6522=DIRECTION('ref_axis',(0.,0.,-1.));
#6523=DIRECTION('',(0.,0.,1.));
#6524=DIRECTION('center_axis',(0.,-1.,0.));
#6525=DIRECTION('ref_axis',(0.,0.,-1.));
#6526=DIRECTION('',(0.,0.,1.));
#6527=DIRECTION('center_axis',(1.,0.,0.));
#6528=DIRECTION('ref_axis',(0.,0.,-1.));
#6529=DIRECTION('center_axis',(1.,0.,0.));
#6530=DIRECTION('ref_axis',(0.,0.,-1.));
#6531=DIRECTION('center_axis',(1.,0.,0.));
#6532=DIRECTION('ref_axis',(0.,0.,-1.));
#6533=DIRECTION('center_axis',(-2.89120579329468E-16,-1.,0.));
#6534=DIRECTION('ref_axis',(1.,-2.89120579329468E-16,0.));
#6535=DIRECTION('',(0.,0.,1.));
#6536=DIRECTION('',(0.,0.,1.));
#6537=DIRECTION('center_axis',(1.,0.,0.));
#6538=DIRECTION('ref_axis',(0.,0.,-1.));
#6539=DIRECTION('center_axis',(1.,0.,0.));
#6540=DIRECTION('ref_axis',(0.,0.,-1.));
#6541=DIRECTION('center_axis',(1.,0.,0.));
#6542=DIRECTION('ref_axis',(0.,0.,-1.));
#6543=DIRECTION('center_axis',(1.,-1.7347234759768E-16,0.));
#6544=DIRECTION('ref_axis',(1.7347234759768E-16,1.,0.));
#6545=DIRECTION('center_axis',(1.,-1.7347234759768E-16,0.));
#6546=DIRECTION('ref_axis',(1.7347234759768E-16,1.,0.));
#6547=DIRECTION('center_axis',(1.,-1.7347234759768E-16,0.));
#6548=DIRECTION('ref_axis',(1.7347234759768E-16,1.,0.));
#6549=DIRECTION('center_axis',(0.,-1.,0.));
#6550=DIRECTION('ref_axis',(0.,0.,-1.));
#6551=DIRECTION('',(0.,0.,1.));
#6552=DIRECTION('',(0.,0.,1.));
#6553=DIRECTION('center_axis',(1.,0.,0.));
#6554=DIRECTION('ref_axis',(0.,0.,-1.));
#6555=DIRECTION('center_axis',(1.,0.,0.));
#6556=DIRECTION('ref_axis',(0.,0.,-1.));
#6557=DIRECTION('center_axis',(1.,0.,0.));
#6558=DIRECTION('ref_axis',(0.,0.,-1.));
#6559=DIRECTION('center_axis',(1.,0.,0.));
#6560=DIRECTION('ref_axis',(0.,0.,-1.));
#6561=DIRECTION('center_axis',(1.,0.,0.));
#6562=DIRECTION('ref_axis',(0.,0.,-1.));
#6563=DIRECTION('center_axis',(1.,0.,0.));
#6564=DIRECTION('ref_axis',(0.,0.,-1.));
#6565=DIRECTION('center_axis',(1.,0.,0.));
#6566=DIRECTION('ref_axis',(0.,0.,-1.));
#6567=DIRECTION('',(1.,0.,0.));
#6568=DIRECTION('center_axis',(-1.,5.78241158658936E-16,0.));
#6569=DIRECTION('ref_axis',(-5.78241158658936E-16,-1.,0.));
#6570=DIRECTION('center_axis',(1.,0.,0.));
#6571=DIRECTION('ref_axis',(0.,0.,-1.));
#6572=DIRECTION('',(1.,0.,0.));
#6573=DIRECTION('center_axis',(-1.,0.,0.));
#6574=DIRECTION('ref_axis',(0.,0.,1.));
#6575=DIRECTION('center_axis',(1.,0.,0.));
#6576=DIRECTION('ref_axis',(0.,0.,-1.));
#6577=DIRECTION('',(1.,0.,0.));
#6578=DIRECTION('center_axis',(-1.,0.,0.));
#6579=DIRECTION('ref_axis',(0.,0.,1.));
#6580=DIRECTION('center_axis',(1.,0.,0.));
#6581=DIRECTION('ref_axis',(0.,0.,-1.));
#6582=DIRECTION('',(1.,0.,0.));
#6583=DIRECTION('center_axis',(1.,0.,0.));
#6584=DIRECTION('ref_axis',(0.,0.,-1.));
#6585=DIRECTION('center_axis',(1.,0.,0.));
#6586=DIRECTION('ref_axis',(0.,0.,-1.));
#6587=DIRECTION('',(1.,0.,0.));
#6588=DIRECTION('center_axis',(1.,-2.89120579329468E-16,0.));
#6589=DIRECTION('ref_axis',(2.89120579329468E-16,1.,0.));
#6590=DIRECTION('center_axis',(1.,0.,0.));
#6591=DIRECTION('ref_axis',(0.,0.,-1.));
#6592=DIRECTION('',(1.,0.,0.));
#6593=DIRECTION('center_axis',(1.,-2.89120579329468E-16,0.));
#6594=DIRECTION('ref_axis',(2.89120579329468E-16,1.,0.));
#6595=DIRECTION('center_axis',(1.,0.,0.));
#6596=DIRECTION('ref_axis',(0.,0.,-1.));
#6597=DIRECTION('',(1.,0.,0.));
#6598=DIRECTION('center_axis',(1.,0.,0.));
#6599=DIRECTION('ref_axis',(0.,0.,-1.));
#6600=DIRECTION('center_axis',(1.,0.,0.));
#6601=DIRECTION('ref_axis',(0.,0.,-1.));
#6602=DIRECTION('',(1.,0.,0.));
#6603=DIRECTION('center_axis',(-1.,0.,0.));
#6604=DIRECTION('ref_axis',(0.,0.,1.));
#6605=DIRECTION('center_axis',(1.,0.,0.));
#6606=DIRECTION('ref_axis',(0.,0.,-1.));
#6607=DIRECTION('center_axis',(1.,0.,0.));
#6608=DIRECTION('ref_axis',(0.,0.,-1.));
#6609=DIRECTION('',(0.,0.,-1.));
#6610=DIRECTION('',(0.,-1.,0.));
#6611=DIRECTION('center_axis',(0.,1.,0.));
#6612=DIRECTION('ref_axis',(0.,0.,1.));
#6613=DIRECTION('',(-1.,0.,0.));
#6614=DIRECTION('',(0.,0.,-1.));
#6615=DIRECTION('',(1.,0.,0.));
#6616=DIRECTION('center_axis',(1.,0.,0.));
#6617=DIRECTION('ref_axis',(0.,0.,-1.));
#6618=DIRECTION('center_axis',(1.,0.,0.));
#6619=DIRECTION('ref_axis',(0.,0.,-1.));
#6620=DIRECTION('',(0.,-1.,0.));
#6621=DIRECTION('center_axis',(0.,1.,0.));
#6622=DIRECTION('ref_axis',(0.,0.,1.));
#6623=DIRECTION('',(-1.,0.,0.));
#6624=DIRECTION('',(0.,0.,-1.));
#6625=DIRECTION('',(1.,0.,0.));
#6626=DIRECTION('center_axis',(1.,0.,0.));
#6627=DIRECTION('ref_axis',(0.,0.,-1.));
#6628=DIRECTION('center_axis',(1.,0.,0.));
#6629=DIRECTION('ref_axis',(0.,0.,-1.));
#6630=DIRECTION('',(0.,-1.,0.));
#6631=DIRECTION('center_axis',(-1.,0.,0.));
#6632=DIRECTION('ref_axis',(0.,0.,1.));
#6633=DIRECTION('center_axis',(-1.,0.,0.));
#6634=DIRECTION('ref_axis',(0.,0.,1.));
#6635=DIRECTION('center_axis',(1.,0.,0.));
#6636=DIRECTION('ref_axis',(0.,0.,-1.));
#6637=DIRECTION('center_axis',(1.,0.,0.));
#6638=DIRECTION('ref_axis',(0.,0.,-1.));
#6639=DIRECTION('',(0.,0.,-1.));
#6640=DIRECTION('',(0.,-1.,0.));
#6641=DIRECTION('center_axis',(-2.89120579329468E-16,1.,0.));
#6642=DIRECTION('ref_axis',(-1.,-2.89120579329468E-16,0.));
#6643=DIRECTION('',(-1.,0.,0.));
#6644=DIRECTION('',(1.,2.89120579329468E-16,0.));
#6645=DIRECTION('center_axis',(1.,0.,0.));
#6646=DIRECTION('ref_axis',(0.,0.,-1.));
#6647=DIRECTION('center_axis',(1.,0.,0.));
#6648=DIRECTION('ref_axis',(0.,0.,-1.));
#6649=DIRECTION('',(0.,0.,-1.));
#6650=DIRECTION('',(0.,-1.,0.));
#6651=DIRECTION('center_axis',(0.,1.,0.));
#6652=DIRECTION('ref_axis',(0.,0.,1.));
#6653=DIRECTION('',(-1.,0.,0.));
#6654=DIRECTION('',(0.,0.,-1.));
#6655=DIRECTION('',(1.,0.,0.));
#6656=DIRECTION('center_axis',(1.,0.,0.));
#6657=DIRECTION('ref_axis',(0.,0.,-1.));
#6658=DIRECTION('center_axis',(1.,0.,0.));
#6659=DIRECTION('ref_axis',(0.,0.,-1.));
#6660=DIRECTION('',(0.,-1.,0.));
#6661=DIRECTION('center_axis',(0.,1.,0.));
#6662=DIRECTION('ref_axis',(0.,0.,1.));
#6663=DIRECTION('',(-1.,0.,0.));
#6664=DIRECTION('center_axis',(0.,1.,0.));
#6665=DIRECTION('ref_axis',(0.,0.,1.));
#6666=DIRECTION('',(-1.,0.,0.));
#6667=DIRECTION('center_axis',(0.,1.,0.));
#6668=DIRECTION('ref_axis',(0.,0.,1.));
#6669=DIRECTION('',(-1.,0.,0.));
#6670=DIRECTION('center_axis',(0.,0.,1.));
#6671=DIRECTION('ref_axis',(1.,0.,0.));
#6672=DIRECTION('',(-1.,0.,0.));
#6673=DIRECTION('',(-1.,0.,0.));
#6674=DIRECTION('',(-1.,0.,0.));
#6675=DIRECTION('',(-1.,0.,0.));
#6676=DIRECTION('',(-1.,0.,0.));
#6677=DIRECTION('center_axis',(-1.,0.,0.));
#6678=DIRECTION('ref_axis',(0.,5.66553889764798E-16,-1.));
#6679=DIRECTION('center_axis',(1.,0.,0.));
#6680=DIRECTION('ref_axis',(0.,0.,-1.));
#6681=DIRECTION('',(-1.,0.,0.));
#6682=DIRECTION('center_axis',(1.,0.,0.));
#6683=DIRECTION('ref_axis',(0.,0.,-1.));
#6684=DIRECTION('',(-1.,0.,0.));
#6685=DIRECTION('',(-1.,0.,0.));
#6686=DIRECTION('center_axis',(1.,0.,0.));
#6687=DIRECTION('ref_axis',(0.,0.,-1.));
#6688=DIRECTION('',(-1.,0.,0.));
#6689=DIRECTION('center_axis',(1.,0.,0.));
#6690=DIRECTION('ref_axis',(0.,0.,-1.));
#6691=DIRECTION('',(-1.,0.,0.));
#6692=DIRECTION('center_axis',(1.,1.7347234759768E-16,0.));
#6693=DIRECTION('ref_axis',(-1.7347234759768E-16,1.,0.));
#6694=DIRECTION('',(-1.,0.,0.));
#6695=DIRECTION('center_axis',(1.,0.,0.));
#6696=DIRECTION('ref_axis',(0.,0.,-1.));
#6697=DIRECTION('',(-1.,0.,0.));
#6698=DIRECTION('center_axis',(-1.,-1.7347234759768E-16,0.));
#6699=DIRECTION('ref_axis',(1.7347234759768E-16,-1.,0.));
#6700=DIRECTION('',(-1.,0.,0.));
#6701=DIRECTION('center_axis',(-1.,0.,0.));
#6702=DIRECTION('ref_axis',(0.,0.,1.));
#6703=DIRECTION('',(-1.,0.,0.));
#6704=DIRECTION('center_axis',(1.,0.,0.));
#6705=DIRECTION('ref_axis',(0.,0.,-1.));
#6706=DIRECTION('',(-1.,0.,0.));
#6707=DIRECTION('center_axis',(1.,1.7347234759768E-16,0.));
#6708=DIRECTION('ref_axis',(-1.7347234759768E-16,1.,0.));
#6709=DIRECTION('center_axis',(1.,0.,0.));
#6710=DIRECTION('ref_axis',(0.,0.,-1.));
#6711=DIRECTION('',(-1.,0.,0.));
#6712=DIRECTION('center_axis',(1.,0.,0.));
#6713=DIRECTION('ref_axis',(0.,0.,-1.));
#6714=DIRECTION('',(-1.,0.,0.));
#6715=DIRECTION('',(-1.,0.,0.));
#6716=DIRECTION('center_axis',(1.,0.,0.));
#6717=DIRECTION('ref_axis',(0.,0.,-1.));
#6718=DIRECTION('',(-1.,0.,0.));
#6719=DIRECTION('center_axis',(1.,0.,0.));
#6720=DIRECTION('ref_axis',(0.,0.,-1.));
#6721=DIRECTION('center_axis',(1.,0.,0.));
#6722=DIRECTION('ref_axis',(0.,0.,-1.));
#6723=DIRECTION('',(-1.,0.,0.));
#6724=DIRECTION('center_axis',(1.,0.,0.));
#6725=DIRECTION('ref_axis',(0.,0.,-1.));
#6726=DIRECTION('',(-1.,0.,0.));
#6727=DIRECTION('center_axis',(0.,1.,0.));
#6728=DIRECTION('ref_axis',(0.,0.,1.));
#6729=DIRECTION('',(0.,0.,-1.));
#6730=DIRECTION('',(0.,0.,-1.));
#6731=DIRECTION('center_axis',(1.,0.,0.));
#6732=DIRECTION('ref_axis',(0.,0.,-1.));
#6733=DIRECTION('center_axis',(1.,0.,0.));
#6734=DIRECTION('ref_axis',(0.,0.,-1.));
#6735=DIRECTION('',(0.,0.,-1.));
#6736=DIRECTION('center_axis',(1.,0.,0.));
#6737=DIRECTION('ref_axis',(0.,0.,-1.));
#6738=DIRECTION('center_axis',(0.,1.,0.));
#6739=DIRECTION('ref_axis',(0.,0.,1.));
#6740=DIRECTION('',(0.,0.,-1.));
#6741=DIRECTION('',(1.,0.,0.));
#6742=DIRECTION('',(-1.,0.,0.));
#6743=DIRECTION('center_axis',(1.,0.,0.));
#6744=DIRECTION('ref_axis',(0.,0.,-1.));
#6745=DIRECTION('center_axis',(1.,0.,0.));
#6746=DIRECTION('ref_axis',(0.,0.,-1.));
#6747=DIRECTION('center_axis',(1.,0.,0.));
#6748=DIRECTION('ref_axis',(0.,0.,-1.));
#6749=DIRECTION('center_axis',(0.,1.,0.));
#6750=DIRECTION('ref_axis',(0.,0.,1.));
#6751=DIRECTION('',(0.,0.,-1.));
#6752=DIRECTION('',(1.,0.,0.));
#6753=DIRECTION('',(0.,0.,-1.));
#6754=DIRECTION('',(1.,0.,0.));
#6755=DIRECTION('center_axis',(1.,0.,0.));
#6756=DIRECTION('ref_axis',(0.,0.,-1.));
#6757=DIRECTION('center_axis',(1.,0.,0.));
#6758=DIRECTION('ref_axis',(0.,0.,-1.));
#6759=DIRECTION('',(0.,0.,-1.));
#6760=DIRECTION('center_axis',(1.,0.,0.));
#6761=DIRECTION('ref_axis',(0.,0.,-1.));
#6762=DIRECTION('center_axis',(0.,1.,0.));
#6763=DIRECTION('ref_axis',(0.,0.,1.));
#6764=DIRECTION('',(0.,0.,-1.));
#6765=DIRECTION('center_axis',(1.,0.,0.));
#6766=DIRECTION('ref_axis',(0.,0.,-1.));
#6767=DIRECTION('center_axis',(1.,0.,0.));
#6768=DIRECTION('ref_axis',(0.,0.,-1.));
#6769=DIRECTION('center_axis',(1.,0.,0.));
#6770=DIRECTION('ref_axis',(0.,0.,-1.));
#6771=DIRECTION('center_axis',(0.,1.,0.));
#6772=DIRECTION('ref_axis',(0.,0.,1.));
#6773=DIRECTION('',(0.,0.,-1.));
#6774=DIRECTION('',(0.,0.,-1.));
#6775=DIRECTION('center_axis',(1.,0.,0.));
#6776=DIRECTION('ref_axis',(0.,0.,-1.));
#6777=DIRECTION('center_axis',(1.,0.,0.));
#6778=DIRECTION('ref_axis',(0.,0.,-1.));
#6779=DIRECTION('',(0.,0.,-1.));
#6780=DIRECTION('center_axis',(1.,0.,0.));
#6781=DIRECTION('ref_axis',(0.,0.,-1.));
#6782=DIRECTION('center_axis',(0.,1.,0.));
#6783=DIRECTION('ref_axis',(0.,0.,1.));
#6784=DIRECTION('',(0.,0.,-1.));
#6785=DIRECTION('',(1.,0.,0.));
#6786=DIRECTION('',(-1.,0.,0.));
#6787=DIRECTION('center_axis',(1.,0.,0.));
#6788=DIRECTION('ref_axis',(0.,0.,-1.));
#6789=DIRECTION('center_axis',(1.,0.,0.));
#6790=DIRECTION('ref_axis',(0.,0.,-1.));
#6791=DIRECTION('center_axis',(1.,0.,0.));
#6792=DIRECTION('ref_axis',(0.,0.,-1.));
#6793=DIRECTION('center_axis',(0.,1.,0.));
#6794=DIRECTION('ref_axis',(0.,0.,1.));
#6795=DIRECTION('',(0.,0.,-1.));
#6796=DIRECTION('',(1.,0.,0.));
#6797=DIRECTION('',(0.,0.,-1.));
#6798=DIRECTION('',(1.,0.,0.));
#6799=DIRECTION('center_axis',(1.,1.7347234759768E-16,0.));
#6800=DIRECTION('ref_axis',(-1.7347234759768E-16,1.,0.));
#6801=DIRECTION('center_axis',(1.,1.7347234759768E-16,0.));
#6802=DIRECTION('ref_axis',(-1.7347234759768E-16,1.,0.));
#6803=DIRECTION('',(0.,0.,-1.));
#6804=DIRECTION('center_axis',(1.,1.7347234759768E-16,0.));
#6805=DIRECTION('ref_axis',(-1.7347234759768E-16,1.,0.));
#6806=DIRECTION('center_axis',(-2.89120579329468E-16,1.,0.));
#6807=DIRECTION('ref_axis',(-1.,-2.89120579329468E-16,0.));
#6808=DIRECTION('',(0.,0.,-1.));
#6809=DIRECTION('center_axis',(1.,0.,0.));
#6810=DIRECTION('ref_axis',(0.,0.,-1.));
#6811=DIRECTION('center_axis',(1.,0.,0.));
#6812=DIRECTION('ref_axis',(0.,0.,-1.));
#6813=DIRECTION('center_axis',(1.,0.,0.));
#6814=DIRECTION('ref_axis',(0.,0.,-1.));
#6815=DIRECTION('center_axis',(0.,-1.,0.));
#6816=DIRECTION('ref_axis',(0.,0.,-1.));
#6817=DIRECTION('',(0.,0.,-1.));
#6818=DIRECTION('',(-1.,0.,0.));
#6819=DIRECTION('',(0.,0.,-1.));
#6820=DIRECTION('',(1.,0.,0.));
#6821=DIRECTION('center_axis',(-1.,0.,0.));
#6822=DIRECTION('ref_axis',(0.,0.,1.));
#6823=DIRECTION('center_axis',(-1.,0.,0.));
#6824=DIRECTION('ref_axis',(0.,0.,1.));
#6825=DIRECTION('',(0.,0.,-1.));
#6826=DIRECTION('center_axis',(-1.,0.,0.));
#6827=DIRECTION('ref_axis',(0.,0.,1.));
#6828=DIRECTION('center_axis',(0.,-1.,0.));
#6829=DIRECTION('ref_axis',(0.,0.,-1.));
#6830=DIRECTION('',(0.,0.,-1.));
#6831=DIRECTION('center_axis',(-1.,-1.7347234759768E-16,0.));
#6832=DIRECTION('ref_axis',(1.7347234759768E-16,-1.,0.));
#6833=DIRECTION('center_axis',(-1.,-1.7347234759768E-16,0.));
#6834=DIRECTION('ref_axis',(1.7347234759768E-16,-1.,0.));
#6835=DIRECTION('center_axis',(-1.,-1.7347234759768E-16,0.));
#6836=DIRECTION('ref_axis',(1.7347234759768E-16,-1.,0.));
#6837=DIRECTION('center_axis',(0.,1.,0.));
#6838=DIRECTION('ref_axis',(0.,0.,1.));
#6839=DIRECTION('',(0.,0.,-1.));
#6840=DIRECTION('',(1.,0.,0.));
#6841=DIRECTION('',(0.,0.,-1.));
#6842=DIRECTION('',(1.,0.,0.));
#6843=DIRECTION('center_axis',(1.,0.,0.));
#6844=DIRECTION('ref_axis',(0.,0.,-1.));
#6845=DIRECTION('center_axis',(1.,0.,0.));
#6846=DIRECTION('ref_axis',(0.,0.,-1.));
#6847=DIRECTION('',(0.,0.,-1.));
#6848=DIRECTION('center_axis',(1.,0.,0.));
#6849=DIRECTION('ref_axis',(0.,0.,-1.));
#6850=DIRECTION('center_axis',(0.,1.,0.));
#6851=DIRECTION('ref_axis',(0.,0.,1.));
#6852=DIRECTION('',(0.,0.,-1.));
#6853=DIRECTION('center_axis',(1.,1.7347234759768E-16,0.));
#6854=DIRECTION('ref_axis',(-1.7347234759768E-16,1.,0.));
#6855=DIRECTION('center_axis',(1.,1.7347234759768E-16,0.));
#6856=DIRECTION('ref_axis',(-1.7347234759768E-16,1.,0.));
#6857=DIRECTION('center_axis',(1.,1.7347234759768E-16,0.));
#6858=DIRECTION('ref_axis',(-1.7347234759768E-16,1.,0.));
#6859=DIRECTION('center_axis',(0.,1.,0.));
#6860=DIRECTION('ref_axis',(0.,0.,1.));
#6861=DIRECTION('',(0.,0.,-1.));
#6862=DIRECTION('',(1.,0.,0.));
#6863=DIRECTION('',(0.,0.,-1.));
#6864=DIRECTION('',(1.,0.,0.));
#6865=DIRECTION('center_axis',(1.,0.,0.));
#6866=DIRECTION('ref_axis',(0.,0.,-1.));
#6867=DIRECTION('center_axis',(1.,0.,0.));
#6868=DIRECTION('ref_axis',(0.,0.,-1.));
#6869=DIRECTION('',(0.,0.,-1.));
#6870=DIRECTION('center_axis',(1.,0.,0.));
#6871=DIRECTION('ref_axis',(0.,0.,-1.));
#6872=DIRECTION('center_axis',(0.,1.,0.));
#6873=DIRECTION('ref_axis',(0.,0.,1.));
#6874=DIRECTION('',(0.,0.,-1.));
#6875=DIRECTION('center_axis',(1.,0.,0.));
#6876=DIRECTION('ref_axis',(0.,0.,-1.));
#6877=DIRECTION('center_axis',(1.,0.,0.));
#6878=DIRECTION('ref_axis',(0.,0.,-1.));
#6879=DIRECTION('center_axis',(1.,0.,0.));
#6880=DIRECTION('ref_axis',(0.,0.,-1.));
#6881=DIRECTION('center_axis',(0.,1.,0.));
#6882=DIRECTION('ref_axis',(0.,0.,1.));
#6883=DIRECTION('',(0.,0.,-1.));
#6884=DIRECTION('',(0.,0.,-1.));
#6885=DIRECTION('center_axis',(1.,0.,0.));
#6886=DIRECTION('ref_axis',(0.,0.,-1.));
#6887=DIRECTION('center_axis',(1.,0.,0.));
#6888=DIRECTION('ref_axis',(0.,0.,-1.));
#6889=DIRECTION('',(0.,0.,-1.));
#6890=DIRECTION('center_axis',(1.,0.,0.));
#6891=DIRECTION('ref_axis',(0.,0.,-1.));
#6892=DIRECTION('center_axis',(-5.78241158658936E-16,1.,0.));
#6893=DIRECTION('ref_axis',(-1.,-5.78241158658936E-16,0.));
#6894=DIRECTION('',(0.,0.,-1.));
#6895=DIRECTION('',(1.,5.78241158658936E-16,0.));
#6896=DIRECTION('',(-1.,-5.78241158658936E-16,0.));
#6897=DIRECTION('center_axis',(1.,0.,0.));
#6898=DIRECTION('ref_axis',(0.,0.,-1.));
#6899=DIRECTION('center_axis',(1.,0.,0.));
#6900=DIRECTION('ref_axis',(0.,0.,-1.));
#6901=DIRECTION('center_axis',(1.,0.,0.));
#6902=DIRECTION('ref_axis',(0.,0.,-1.));
#6903=DIRECTION('center_axis',(1.,0.,0.));
#6904=DIRECTION('ref_axis',(0.,0.,-1.));
#6905=DIRECTION('center_axis',(1.,0.,0.));
#6906=DIRECTION('ref_axis',(0.,0.,-1.));
#6907=DIRECTION('center_axis',(1.,5.78241158658936E-16,0.));
#6908=DIRECTION('ref_axis',(-5.78241158658936E-16,1.,0.));
#6909=DIRECTION('center_axis',(1.,0.,0.));
#6910=DIRECTION('ref_axis',(0.,0.,-1.));
#6911=DIRECTION('center_axis',(-1.,0.,0.));
#6912=DIRECTION('ref_axis',(0.,0.,1.));
#6913=DIRECTION('center_axis',(-1.,0.,0.));
#6914=DIRECTION('ref_axis',(0.,0.,1.));
#6915=DIRECTION('center_axis',(-1.,0.,0.));
#6916=DIRECTION('ref_axis',(0.,0.,1.));
#6917=DIRECTION('center_axis',(-1.,0.,0.));
#6918=DIRECTION('ref_axis',(0.,0.,1.));
#6919=DIRECTION('center_axis',(-1.,0.,0.));
#6920=DIRECTION('ref_axis',(0.,0.,1.));
#6921=DIRECTION('center_axis',(-1.,0.,0.));
#6922=DIRECTION('ref_axis',(0.,0.,1.));
#6923=DIRECTION('center_axis',(-1.,0.,0.));
#6924=DIRECTION('ref_axis',(0.,0.,1.));
#6925=DIRECTION('center_axis',(-1.,0.,0.));
#6926=DIRECTION('ref_axis',(0.,0.,1.));
#6927=DIRECTION('center_axis',(-1.,0.,0.));
#6928=DIRECTION('ref_axis',(0.,0.,1.));
#6929=DIRECTION('center_axis',(-1.,0.,0.));
#6930=DIRECTION('ref_axis',(0.,0.,1.));
#6931=DIRECTION('center_axis',(-1.,0.,0.));
#6932=DIRECTION('ref_axis',(0.,0.,1.));
#6933=DIRECTION('center_axis',(-1.,0.,0.));
#6934=DIRECTION('ref_axis',(0.,0.,1.));
#6935=DIRECTION('center_axis',(-1.,0.,0.));
#6936=DIRECTION('ref_axis',(0.,0.,1.));
#6937=DIRECTION('axis',(0.,0.,1.));
#6938=DIRECTION('refdir',(1.,0.,0.));
#6939=DIRECTION('center_axis',(1.,-1.34352275263155E-12,-2.55900709108327E-25));
#6940=DIRECTION('ref_axis',(1.34352275263155E-12,1.,-8.56382735160077E-17));
#6941=DIRECTION('center_axis',(1.,-1.34352275263155E-12,-2.55900709108327E-25));
#6942=DIRECTION('ref_axis',(-1.34352275263155E-12,-1.,-7.01978908408492E-15));
#6943=DIRECTION('',(1.34352275940781E-12,1.,-8.56382735160077E-17));
#6944=DIRECTION('center_axis',(1.,-1.34352275940781E-12,6.7760076773746E-21));
#6945=DIRECTION('ref_axis',(6.776017108621E-21,7.01978908408497E-15,-1.));
#6946=DIRECTION('',(-4.77281939087608E-22,8.56382735160077E-17,1.));
#6947=DIRECTION('center_axis',(1.,-1.33641732527395E-12,-2.55901399361619E-25));
#6948=DIRECTION('ref_axis',(1.33641732527395E-12,1.,-8.56382735160077E-17));
#6949=DIRECTION('',(-1.35150638374886E-12,-1.,8.56382735160077E-17));
#6950=DIRECTION('center_axis',(1.,-1.34352275940781E-12,6.7760076773746E-21));
#6951=DIRECTION('ref_axis',(-6.77602665492437E-21,-1.4125216441686E-14,
1.));
#6952=DIRECTION('',(4.23489977076173E-21,-6.74697642126694E-15,-1.));
#6953=DIRECTION('center_axis',(-1.,1.34352275940781E-12,2.55900709108327E-25));
#6954=DIRECTION('ref_axis',(-2.56015766077872E-25,-8.56382735160077E-17,
-1.));
#6955=DIRECTION('center_axis',(1.,-1.34352275940781E-12,-7.10542735785685E-15));
#6956=DIRECTION('ref_axis',(7.10542735785219E-15,-3.46707540529401E-15,
1.));
#6957=DIRECTION('',(9.69167893318796E-22,9.30874939302446E-16,-1.));
#6958=DIRECTION('center_axis',(1.,-1.35062817998915E-12,-2.55950555256775E-25));
#6959=DIRECTION('ref_axis',(-1.35062817998915E-12,-1.,-7.01978908408499E-15));
#6960=DIRECTION('center_axis',(-1.,1.34352275263155E-12,2.55900709108327E-25));
#6961=DIRECTION('ref_axis',(1.34352275263155E-12,1.,-8.56382735160077E-17));
#6962=DIRECTION('',(-2.56015784192876E-25,-8.56382735160077E-17,-1.));
#6963=DIRECTION('center_axis',(0.,-1.,8.57182693503055E-17));
#6964=DIRECTION('ref_axis',(0.,-8.57182693503055E-17,-1.));
#6965=DIRECTION('',(0.,-8.57182693503055E-17,-1.));
#6966=DIRECTION('',(-1.,0.,0.));
#6967=DIRECTION('',(-1.,0.,0.));
#6968=DIRECTION('center_axis',(0.,0.,1.));
#6969=DIRECTION('ref_axis',(-1.,0.,0.));
#6970=DIRECTION('',(-1.,0.,0.));
#6971=DIRECTION('',(0.,-1.,0.));
#6972=DIRECTION('',(1.,-1.34336985979644E-12,0.));
#6973=DIRECTION('center_axis',(0.,-1.,6.42887020127291E-17));
#6974=DIRECTION('ref_axis',(0.,-6.42887020127291E-17,-1.));
#6975=DIRECTION('',(-1.,0.,0.));
#6976=DIRECTION('',(0.,-6.42887020127291E-17,-1.));
#6977=DIRECTION('',(1.,-1.34336985979644E-12,0.));
#6978=DIRECTION('center_axis',(0.,1.,-6.42887020127291E-17));
#6979=DIRECTION('ref_axis',(0.,-6.42887020127291E-17,-1.));
#6980=DIRECTION('center_axis',(0.,1.,-6.42887020127291E-17));
#6981=DIRECTION('ref_axis',(0.,-6.42887020127291E-17,-1.));
#6982=DIRECTION('center_axis',(0.,0.,1.));
#6983=DIRECTION('ref_axis',(-1.,0.,0.));
#6984=DIRECTION('',(-1.,0.,0.));
#6985=DIRECTION('',(0.,-1.,0.));
#6986=DIRECTION('',(1.,-1.34336985979644E-12,0.));
#6987=DIRECTION('center_axis',(-1.,0.,0.));
#6988=DIRECTION('ref_axis',(0.,0.,-1.));
#6989=DIRECTION('center_axis',(-1.,0.,0.));
#6990=DIRECTION('ref_axis',(0.,0.,1.));
#6991=DIRECTION('',(-1.,0.,0.));
#6992=DIRECTION('center_axis',(-1.,0.,0.));
#6993=DIRECTION('ref_axis',(0.,0.,1.));
#6994=DIRECTION('center_axis',(0.,-1.,8.57182693503055E-17));
#6995=DIRECTION('ref_axis',(0.,-8.57182693503055E-17,-1.));
#6996=DIRECTION('',(-1.,0.,0.));
#6997=DIRECTION('',(0.,-8.57182693503055E-17,-1.));
#6998=DIRECTION('',(1.,-1.34336985979644E-12,0.));
#6999=DIRECTION('center_axis',(-1.,0.,0.));
#7000=DIRECTION('ref_axis',(0.,0.,-1.));
#7001=DIRECTION('center_axis',(-1.,0.,0.));
#7002=DIRECTION('ref_axis',(0.,0.,1.));
#7003=DIRECTION('',(-1.,0.,0.));
#7004=DIRECTION('center_axis',(-1.,0.,0.));
#7005=DIRECTION('ref_axis',(0.,0.,1.));
#7006=DIRECTION('center_axis',(1.,0.,0.));
#7007=DIRECTION('ref_axis',(0.,-1.,0.));
#7008=DIRECTION('',(0.,-8.57182693503055E-17,-1.));
#7009=DIRECTION('center_axis',(-1.,0.,0.));
#7010=DIRECTION('ref_axis',(0.,0.,1.));
#7011=DIRECTION('center_axis',(-1.,0.,0.));
#7012=DIRECTION('ref_axis',(0.,0.,1.));
#7013=DIRECTION('center_axis',(-1.,0.,0.));
#7014=DIRECTION('ref_axis',(0.,0.,1.));
#7015=DIRECTION('center_axis',(-1.,0.,0.));
#7016=DIRECTION('ref_axis',(0.,0.,1.));
#7017=DIRECTION('center_axis',(-1.,0.,0.));
#7018=DIRECTION('ref_axis',(0.,0.,1.));
#7019=DIRECTION('center_axis',(-1.,0.,0.));
#7020=DIRECTION('ref_axis',(0.,0.,1.));
#7021=DIRECTION('center_axis',(-1.,0.,0.));
#7022=DIRECTION('ref_axis',(0.,0.,1.));
#7023=DIRECTION('center_axis',(-1.,0.,0.));
#7024=DIRECTION('ref_axis',(0.,0.,1.));
#7025=DIRECTION('center_axis',(1.,0.,0.));
#7026=DIRECTION('ref_axis',(0.,-1.,0.));
#7027=DIRECTION('center_axis',(1.,0.,0.));
#7028=DIRECTION('ref_axis',(0.,-1.,0.));
#7029=DIRECTION('center_axis',(-1.,0.,0.));
#7030=DIRECTION('ref_axis',(0.,0.,-1.));
#7031=DIRECTION('center_axis',(1.,0.,0.));
#7032=DIRECTION('ref_axis',(0.,0.,1.));
#7033=DIRECTION('center_axis',(-1.,0.,0.));
#7034=DIRECTION('ref_axis',(0.,0.,-1.));
#7035=DIRECTION('center_axis',(1.,0.,0.));
#7036=DIRECTION('ref_axis',(0.,0.,1.));
#7037=DIRECTION('center_axis',(0.,-1.,8.57182693503055E-17));
#7038=DIRECTION('ref_axis',(-1.,0.,0.));
#7039=DIRECTION('',(1.,-1.34336985979644E-12,0.));
#7040=DIRECTION('center_axis',(0.,1.,-8.57182693503055E-17));
#7041=DIRECTION('ref_axis',(0.,-8.57182693503055E-17,-1.));
#7042=DIRECTION('',(-1.,0.,0.));
#7043=DIRECTION('',(-1.,0.,0.));
#7044=DIRECTION('center_axis',(0.,1.,-8.57182693503055E-17));
#7045=DIRECTION('ref_axis',(0.,-8.57182693503055E-17,-1.));
#7046=DIRECTION('center_axis',(0.,1.,-8.57182693503055E-17));
#7047=DIRECTION('ref_axis',(0.,-8.57182693503055E-17,-1.));
#7048=DIRECTION('',(1.,-1.34336985979644E-12,0.));
#7049=DIRECTION('center_axis',(0.,-1.,8.57182693503055E-17));
#7050=DIRECTION('ref_axis',(0.,-8.57182693503055E-17,-1.));
#7051=DIRECTION('',(0.,-1.,8.57182693503055E-17));
#7052=DIRECTION('center_axis',(0.,-1.,8.57182693503055E-17));
#7053=DIRECTION('ref_axis',(0.,-8.57182693503055E-17,-1.));
#7054=DIRECTION('',(0.,-1.,8.57182693503055E-17));
#7055=DIRECTION('center_axis',(1.,0.,0.));
#7056=DIRECTION('ref_axis',(0.,0.,1.));
#7057=DIRECTION('',(1.,-1.34336985979644E-12,0.));
#7058=DIRECTION('center_axis',(-1.,0.,0.));
#7059=DIRECTION('ref_axis',(0.,0.,-1.));
#7060=DIRECTION('center_axis',(-1.,0.,0.));
#7061=DIRECTION('ref_axis',(0.,0.,-1.));
#7062=DIRECTION('',(1.,-1.34336985979644E-12,0.));
#7063=DIRECTION('center_axis',(1.,0.,0.));
#7064=DIRECTION('ref_axis',(0.,0.,1.));
#7065=DIRECTION('axis',(0.,0.,1.));
#7066=DIRECTION('refdir',(1.,0.,0.));
#7067=DIRECTION('center_axis',(0.,0.,-1.));
#7068=DIRECTION('ref_axis',(-1.,0.,0.));
#7069=DIRECTION('center_axis',(0.,0.,1.));
#7070=DIRECTION('ref_axis',(1.,0.,0.));
#7071=DIRECTION('',(0.,0.,1.));
#7072=DIRECTION('center_axis',(0.,0.,1.));
#7073=DIRECTION('ref_axis',(1.,0.,0.));
#7074=DIRECTION('center_axis',(0.,0.,1.));
#7075=DIRECTION('ref_axis',(1.,0.,0.));
#7076=DIRECTION('center_axis',(0.,0.,1.));
#7077=DIRECTION('ref_axis',(1.,0.,0.));
#7078=DIRECTION('center_axis',(0.,0.,1.));
#7079=DIRECTION('ref_axis',(1.,0.,0.));
#7080=DIRECTION('center_axis',(0.,0.,1.));
#7081=DIRECTION('ref_axis',(1.,0.,0.));
#7082=DIRECTION('center_axis',(0.,0.,1.));
#7083=DIRECTION('ref_axis',(1.,0.,0.));
#7084=DIRECTION('center_axis',(0.,0.,1.));
#7085=DIRECTION('ref_axis',(1.,0.,0.));
#7086=DIRECTION('center_axis',(0.,0.,1.));
#7087=DIRECTION('ref_axis',(1.,0.,0.));
#7088=DIRECTION('center_axis',(1.22464679914735E-16,-1.,0.));
#7089=DIRECTION('ref_axis',(-1.,-1.22464679914735E-16,0.));
#7090=DIRECTION('center_axis',(0.,0.,1.));
#7091=DIRECTION('ref_axis',(1.,0.,0.));
#7092=DIRECTION('center_axis',(1.22464679914735E-16,-1.,0.));
#7093=DIRECTION('ref_axis',(-1.,-1.22464679914735E-16,0.));
#7094=DIRECTION('axis',(0.,0.,1.));
#7095=DIRECTION('refdir',(1.,0.,0.));
#7096=DIRECTION('axis',(0.,0.,1.));
#7097=DIRECTION('refdir',(1.,0.,0.));
#7098=DIRECTION('center_axis',(0.,-1.,0.));
#7099=DIRECTION('ref_axis',(0.,0.,-1.));
#7100=DIRECTION('center_axis',(0.,1.,0.));
#7101=DIRECTION('ref_axis',(1.,0.,0.));
#7102=DIRECTION('center_axis',(0.,1.,0.));
#7103=DIRECTION('ref_axis',(1.,0.,0.));
#7104=DIRECTION('center_axis',(0.,1.,0.));
#7105=DIRECTION('ref_axis',(0.,0.,1.));
#7106=DIRECTION('center_axis',(0.,1.,0.));
#7107=DIRECTION('ref_axis',(1.,0.,0.));
#7108=DIRECTION('',(0.,-1.,0.));
#7109=DIRECTION('center_axis',(0.,1.,0.));
#7110=DIRECTION('ref_axis',(1.,0.,0.));
#7111=DIRECTION('center_axis',(0.,1.,0.));
#7112=DIRECTION('ref_axis',(1.,0.,0.));
#7113=DIRECTION('center_axis',(0.,1.,0.));
#7114=DIRECTION('ref_axis',(0.,0.,1.));
#7115=DIRECTION('',(0.,1.,0.));
#7116=DIRECTION('axis',(0.,0.,1.));
#7117=DIRECTION('refdir',(1.,0.,0.));
#7118=DIRECTION('center_axis',(0.,-1.,0.));
#7119=DIRECTION('ref_axis',(0.,0.,-1.));
#7120=DIRECTION('center_axis',(0.,1.,0.));
#7121=DIRECTION('ref_axis',(0.,0.,-1.));
#7122=DIRECTION('',(-8.65956056235503E-17,-0.70710678118654,0.707106781186555));
#7123=DIRECTION('center_axis',(0.,-1.,0.));
#7124=DIRECTION('ref_axis',(0.,0.,-1.));
#7125=DIRECTION('center_axis',(0.,1.,0.));
#7126=DIRECTION('ref_axis',(0.,0.,-1.));
#7127=DIRECTION('center_axis',(0.,-1.,0.));
#7128=DIRECTION('ref_axis',(0.,0.,-1.));
#7129=DIRECTION('center_axis',(0.,1.,0.));
#7130=DIRECTION('ref_axis',(0.,0.,-1.));
#7131=DIRECTION('center_axis',(0.,1.,0.));
#7132=DIRECTION('ref_axis',(0.,0.,1.));
#7133=DIRECTION('',(0.,1.,0.));
#7134=DIRECTION('center_axis',(0.,1.,0.));
#7135=DIRECTION('ref_axis',(1.,0.,0.));
#7136=DIRECTION('center_axis',(0.,1.,0.));
#7137=DIRECTION('ref_axis',(0.,0.,-1.));
#7138=DIRECTION('center_axis',(0.,-1.,0.));
#7139=DIRECTION('ref_axis',(0.,0.,-1.));
#7140=DIRECTION('',(-8.65956056235493E-17,-0.707106781186548,-0.707106781186547));
#7141=DIRECTION('center_axis',(0.,-1.,0.));
#7142=DIRECTION('ref_axis',(0.,0.,-1.));
#7143=DIRECTION('center_axis',(0.,1.,0.));
#7144=DIRECTION('ref_axis',(0.,0.,1.));
#7145=DIRECTION('center_axis',(0.,1.,0.));
#7146=DIRECTION('ref_axis',(1.,0.,0.));
#7147=DIRECTION('',(0.,-1.,0.));
#7148=DIRECTION('center_axis',(0.,1.,0.));
#7149=DIRECTION('ref_axis',(0.,0.,-1.));
#7150=DIRECTION('center_axis',(0.,-1.,0.));
#7151=DIRECTION('ref_axis',(0.,0.,-1.));
#7152=DIRECTION('',(8.65956056235503E-17,0.70710678118654,0.707106781186555));
#7153=DIRECTION('center_axis',(0.,1.,0.));
#7154=DIRECTION('ref_axis',(0.,0.,-1.));
#7155=DIRECTION('center_axis',(0.,-1.,0.));
#7156=DIRECTION('ref_axis',(0.,0.,-1.));
#7157=DIRECTION('center_axis',(0.,1.,0.));
#7158=DIRECTION('ref_axis',(1.,0.,0.));
#7159=DIRECTION('center_axis',(0.,-1.,0.));
#7160=DIRECTION('ref_axis',(0.,0.,-1.));
#7161=DIRECTION('center_axis',(0.,1.,0.));
#7162=DIRECTION('ref_axis',(0.,0.,1.));
#7163=DIRECTION('center_axis',(0.,1.,0.));
#7164=DIRECTION('ref_axis',(1.,0.,0.));
#7165=DIRECTION('',(0.,1.,0.));
#7166=DIRECTION('center_axis',(0.,-1.,0.));
#7167=DIRECTION('ref_axis',(0.,0.,-1.));
#7168=DIRECTION('center_axis',(0.,1.,0.));
#7169=DIRECTION('ref_axis',(0.,0.,-1.));
#7170=DIRECTION('',(8.65956056235493E-17,0.707106781186548,-0.707106781186547));
#7171=DIRECTION('center_axis',(0.,1.,0.));
#7172=DIRECTION('ref_axis',(0.,0.,-1.));
#7173=DIRECTION('center_axis',(0.,1.,0.));
#7174=DIRECTION('ref_axis',(0.,0.,1.));
#7175=DIRECTION('',(0.,-1.,0.));
#7176=DIRECTION('center_axis',(0.,1.,0.));
#7177=DIRECTION('ref_axis',(1.,0.,0.));
#7178=DIRECTION('center_axis',(0.,-1.,0.));
#7179=DIRECTION('ref_axis',(0.,0.,-1.));
#7180=DIRECTION('center_axis',(0.,1.,0.));
#7181=DIRECTION('ref_axis',(1.,0.,0.));
#7182=DIRECTION('center_axis',(0.,1.,0.));
#7183=DIRECTION('ref_axis',(0.,0.,1.));
#7184=DIRECTION('center_axis',(0.,1.,0.));
#7185=DIRECTION('ref_axis',(1.,0.,0.));
#7186=DIRECTION('',(0.,1.,0.));
#7187=DIRECTION('center_axis',(0.,1.,0.));
#7188=DIRECTION('ref_axis',(1.,0.,0.));
#7189=DIRECTION('center_axis',(0.,1.,0.));
#7190=DIRECTION('ref_axis',(1.,0.,0.));
#7191=DIRECTION('center_axis',(0.,1.,0.));
#7192=DIRECTION('ref_axis',(0.,0.,1.));
#7193=DIRECTION('center_axis',(0.,1.,0.));
#7194=DIRECTION('ref_axis',(1.,0.,0.));
#7195=DIRECTION('',(0.,1.,0.));
#7196=DIRECTION('center_axis',(0.,1.,0.));
#7197=DIRECTION('ref_axis',(0.,0.,1.));
#7198=DIRECTION('center_axis',(0.,1.,0.));
#7199=DIRECTION('ref_axis',(1.,0.,0.));
#7200=DIRECTION('',(-1.93482561475974E-17,0.987440631916705,-0.157990501106673));
#7201=DIRECTION('center_axis',(0.,1.,0.));
#7202=DIRECTION('ref_axis',(0.,0.,1.));
#7203=DIRECTION('center_axis',(0.,1.,0.));
#7204=DIRECTION('ref_axis',(1.,0.,0.));
#7205=DIRECTION('',(0.,1.,0.));
#7206=DIRECTION('center_axis',(0.,-1.,0.));
#7207=DIRECTION('ref_axis',(0.,0.,1.));
#7208=DIRECTION('',(1.93482561475974E-17,-0.987440631916705,-0.157990501106673));
#7209=DIRECTION('center_axis',(0.,1.,0.));
#7210=DIRECTION('ref_axis',(1.,0.,0.));
#7211=DIRECTION('center_axis',(0.,1.,0.));
#7212=DIRECTION('ref_axis',(0.,0.,1.));
#7213=DIRECTION('center_axis',(0.,1.,0.));
#7214=DIRECTION('ref_axis',(1.,0.,0.));
#7215=DIRECTION('',(0.,1.,0.));
#7216=DIRECTION('center_axis',(0.,-1.,0.));
#7217=DIRECTION('ref_axis',(0.,0.,-1.));
#7218=DIRECTION('center_axis',(0.,1.,0.));
#7219=DIRECTION('ref_axis',(1.,0.,0.));
#7220=DIRECTION('center_axis',(0.,1.,0.));
#7221=DIRECTION('ref_axis',(0.,0.,1.));
#7222=DIRECTION('center_axis',(0.,1.,0.));
#7223=DIRECTION('ref_axis',(1.,0.,0.));
#7224=DIRECTION('',(0.,1.,0.));
#7225=DIRECTION('center_axis',(0.,1.,0.));
#7226=DIRECTION('ref_axis',(1.,0.,0.));
#7227=DIRECTION('center_axis',(0.,1.,0.));
#7228=DIRECTION('ref_axis',(1.,0.,0.));
#7229=DIRECTION('center_axis',(0.,1.,0.));
#7230=DIRECTION('ref_axis',(1.,0.,0.));
#7231=DIRECTION('center_axis',(0.,1.,0.));
#7232=DIRECTION('ref_axis',(0.,0.,1.));
#7233=DIRECTION('center_axis',(0.,1.,0.));
#7234=DIRECTION('ref_axis',(1.,0.,0.));
#7235=DIRECTION('',(0.,-1.,0.));
#7236=DIRECTION('center_axis',(0.,-1.,0.));
#7237=DIRECTION('ref_axis',(0.,0.,-1.));
#7238=DIRECTION('center_axis',(0.,1.,0.));
#7239=DIRECTION('ref_axis',(1.,0.,0.));
#7240=DIRECTION('center_axis',(0.,1.,0.));
#7241=DIRECTION('ref_axis',(0.,0.,1.));
#7242=DIRECTION('center_axis',(0.,1.,0.));
#7243=DIRECTION('ref_axis',(1.,0.,0.));
#7244=DIRECTION('',(0.,-1.,0.));
#7245=DIRECTION('center_axis',(0.,1.,0.));
#7246=DIRECTION('ref_axis',(1.,0.,0.));
#7247=DIRECTION('center_axis',(0.,1.,0.));
#7248=DIRECTION('ref_axis',(1.,0.,0.));
#7249=DIRECTION('center_axis',(0.,1.,0.));
#7250=DIRECTION('ref_axis',(0.,0.,1.));
#7251=DIRECTION('center_axis',(0.,1.,0.));
#7252=DIRECTION('ref_axis',(1.,0.,0.));
#7253=DIRECTION('',(0.,-1.,0.));
#7254=DIRECTION('center_axis',(0.,-1.,0.));
#7255=DIRECTION('ref_axis',(0.,0.,-1.));
#7256=DIRECTION('axis',(0.,0.,1.));
#7257=DIRECTION('refdir',(1.,0.,0.));
#7258=DIRECTION('center_axis',(0.,-1.,0.));
#7259=DIRECTION('ref_axis',(0.,0.,-1.));
#7260=DIRECTION('center_axis',(0.,1.,0.));
#7261=DIRECTION('ref_axis',(1.,0.,0.));
#7262=DIRECTION('center_axis',(0.,1.,0.));
#7263=DIRECTION('ref_axis',(1.,0.,0.));
#7264=DIRECTION('center_axis',(0.,1.,0.));
#7265=DIRECTION('ref_axis',(0.,0.,1.));
#7266=DIRECTION('center_axis',(0.,1.,0.));
#7267=DIRECTION('ref_axis',(1.,0.,0.));
#7268=DIRECTION('',(0.,-1.,0.));
#7269=DIRECTION('center_axis',(0.,1.,0.));
#7270=DIRECTION('ref_axis',(1.,0.,0.));
#7271=DIRECTION('center_axis',(0.,1.,0.));
#7272=DIRECTION('ref_axis',(1.,0.,0.));
#7273=DIRECTION('center_axis',(0.,1.,0.));
#7274=DIRECTION('ref_axis',(0.,0.,1.));
#7275=DIRECTION('center_axis',(0.,1.,0.));
#7276=DIRECTION('ref_axis',(1.,0.,0.));
#7277=DIRECTION('',(-8.65956056235493E-17,0.707106781186548,-0.707106781186547));
#7278=DIRECTION('center_axis',(0.,1.,0.));
#7279=DIRECTION('ref_axis',(0.,0.,1.));
#7280=DIRECTION('center_axis',(0.,1.,0.));
#7281=DIRECTION('ref_axis',(1.,0.,0.));
#7282=DIRECTION('',(0.,1.,0.));
#7283=DIRECTION('center_axis',(0.,-1.,0.));
#7284=DIRECTION('ref_axis',(0.,0.,-1.));
#7285=DIRECTION('center_axis',(0.,1.,0.));
#7286=DIRECTION('ref_axis',(1.,0.,0.));
#7287=DIRECTION('center_axis',(0.,1.,0.));
#7288=DIRECTION('ref_axis',(0.,0.,1.));
#7289=DIRECTION('',(8.65956056235493E-17,-0.707106781186548,0.707106781186547));
#7290=DIRECTION('axis',(0.,0.,1.));
#7291=DIRECTION('refdir',(1.,0.,0.));
#7292=DIRECTION('center_axis',(0.,-1.,0.));
#7293=DIRECTION('ref_axis',(1.,0.,0.));
#7294=DIRECTION('center_axis',(0.,1.,0.));
#7295=DIRECTION('ref_axis',(1.,0.,0.));
#7296=DIRECTION('center_axis',(0.,1.,0.));
#7297=DIRECTION('ref_axis',(1.,0.,0.));
#7298=DIRECTION('center_axis',(0.,1.,0.));
#7299=DIRECTION('ref_axis',(0.,0.,1.));
#7300=DIRECTION('',(0.,-1.,0.));
#7301=DIRECTION('center_axis',(0.,1.,0.));
#7302=DIRECTION('ref_axis',(1.,0.,0.));
#7303=DIRECTION('center_axis',(0.,1.,0.));
#7304=DIRECTION('ref_axis',(0.,0.,1.));
#7305=DIRECTION('center_axis',(0.,1.,0.));
#7306=DIRECTION('ref_axis',(1.,0.,0.));
#7307=DIRECTION('center_axis',(0.,1.,0.));
#7308=DIRECTION('ref_axis',(0.,0.,1.));
#7309=DIRECTION('',(0.,1.,0.));
#7310=DIRECTION('axis',(0.,0.,1.));
#7311=DIRECTION('refdir',(1.,0.,0.));
#7312=DIRECTION('center_axis',(0.,-1.,0.));
#7313=DIRECTION('ref_axis',(1.,0.,0.));
#7314=DIRECTION('center_axis',(0.,1.,0.));
#7315=DIRECTION('ref_axis',(1.,0.,0.));
#7316=DIRECTION('center_axis',(0.,1.,0.));
#7317=DIRECTION('ref_axis',(1.,0.,0.));
#7318=DIRECTION('center_axis',(0.,1.,0.));
#7319=DIRECTION('ref_axis',(0.,0.,1.));
#7320=DIRECTION('',(0.,-1.,0.));
#7321=DIRECTION('center_axis',(0.,1.,0.));
#7322=DIRECTION('ref_axis',(1.,0.,0.));
#7323=DIRECTION('center_axis',(0.,1.,0.));
#7324=DIRECTION('ref_axis',(0.,0.,1.));
#7325=DIRECTION('center_axis',(0.,1.,0.));
#7326=DIRECTION('ref_axis',(1.,0.,0.));
#7327=DIRECTION('center_axis',(0.,-1.,0.));
#7328=DIRECTION('ref_axis',(0.,0.,1.));
#7329=DIRECTION('center_axis',(0.,1.,0.));
#7330=DIRECTION('ref_axis',(1.,0.,0.));
#7331=DIRECTION('',(8.65956056235493E-17,-0.707106781186548,-0.707106781186547));
#7332=DIRECTION('center_axis',(0.,1.,0.));
#7333=DIRECTION('ref_axis',(0.,0.,1.));
#7334=DIRECTION('',(0.,1.,0.));
#7335=DIRECTION('center_axis',(0.,1.,0.));
#7336=DIRECTION('ref_axis',(1.,0.,0.));
#7337=DIRECTION('center_axis',(0.,-1.,0.));
#7338=DIRECTION('ref_axis',(1.,0.,0.));
#7339=DIRECTION('center_axis',(0.,1.,0.));
#7340=DIRECTION('ref_axis',(1.,0.,0.));
#7341=DIRECTION('center_axis',(0.,-1.,0.));
#7342=DIRECTION('ref_axis',(0.,0.,1.));
#7343=DIRECTION('',(-8.65956056235493E-17,0.707106781186548,0.707106781186547));
#7344=DIRECTION('',(-4.44089213073703E-16,5.29544312316906E-20,1.));
#7345=DIRECTION('',(0.999999998147046,6.0876171481578E-5,4.44089209027163E-16));
#7346=DIRECTION('',(-4.44089213073703E-16,5.29544312316906E-20,1.));
#7347=DIRECTION('',(0.999999998147046,6.0876171481578E-5,4.44089209027163E-16));
#7348=DIRECTION('',(-4.44089213073703E-16,5.29544312316906E-20,1.));
#7349=DIRECTION('',(0.999999998147046,6.0876171481578E-5,4.44089209027163E-16));
#7350=DIRECTION('',(-4.44089213073703E-16,5.29544312316906E-20,1.));
#7351=DIRECTION('',(0.999999998147046,6.0876171481578E-5,4.44089209027163E-16));
#7352=DIRECTION('',(-4.44089213073703E-16,5.29544312316906E-20,1.));
#7353=DIRECTION('',(0.999999998147046,6.0876171481578E-5,4.44089209027163E-16));
#7354=DIRECTION('',(-4.44083994873641E-16,-8.56653147352083E-17,1.));
#7355=DIRECTION('',(0.999999998147046,6.0876171481578E-5,4.44089209027163E-16));
#7356=DIRECTION('',(-1.26994078154953E-15,2.02370814783034E-15,1.));
#7357=DIRECTION('',(0.999999998147046,6.08761714816613E-5,1.26981758359215E-15));
#7358=DIRECTION('',(-4.44083995047419E-16,-8.5665308427967E-17,1.));
#7359=DIRECTION('',(0.999999998147046,6.08761714818278E-5,4.44089209200558E-16));
#7360=DIRECTION('',(0.,0.,1.));
#7361=DIRECTION('',(1.,0.,0.));
#7362=DIRECTION('',(-0.999999998147046,-6.08761714818277E-5,-4.44089209200552E-16));
#7363=DIRECTION('',(-4.44083995040506E-16,-8.56654218933077E-17,1.));
#7364=DIRECTION('',(-6.08761714816129E-5,0.999999998147046,1.17266642485094E-16));
#7365=DIRECTION('',(0.999999998147046,6.08761714816129E-5,4.44448351819699E-16));
#7366=DIRECTION('',(6.08761714816144E-5,-0.999999998147046,-1.17293765838873E-16));
#7367=DIRECTION('',(0.999999998147046,6.08761714816144E-5,4.44089209027163E-16));
#7368=DIRECTION('',(6.08761714815766E-5,-0.999999998147046,5.40668696684198E-20));
#7369=DIRECTION('',(0.999999998147046,6.08761714815766E-5,4.43730067880427E-16));
#7370=DIRECTION('',(-0.999999998147046,-6.0876171481578E-5,-4.44089209027159E-16));
#7371=DIRECTION('',(-4.4408399486875E-16,-8.56653950099378E-17,1.));
#7372=DIRECTION('',(-6.0876171481578E-5,0.999999998147046,-2.69914374984392E-20));
#7373=DIRECTION('',(0.999999998147046,6.0876171481578E-5,4.44089209027163E-16));
#7374=DIRECTION('',(0.948122329809734,5.77180576392101E-5,-0.317905716187659));
#7375=DIRECTION('',(-0.317905711303622,-8.02290542261584E-5,-0.948122329809734));
#7376=DIRECTION('',(-5.77180576416081E-5,0.948122329809733,-0.31790571618766));
#7377=DIRECTION('',(8.02290542278412E-5,-0.317905711303622,-0.948122329809733));
#7378=DIRECTION('',(-5.77180576416346E-5,0.948122329809733,-0.317905716187662));
#7379=DIRECTION('',(8.02290542277628E-5,-0.317905711303625,-0.948122329809733));
#7380=DIRECTION('',(-5.77180576416019E-5,0.948122329809733,-0.31790571618766));
#7381=DIRECTION('',(8.02290542280683E-5,-0.317905711303623,-0.948122329809733));
#7382=DIRECTION('',(-5.77180576416926E-5,0.948122329809732,-0.317905716187663));
#7383=DIRECTION('',(8.02290542277978E-5,-0.317905711303625,-0.948122329809732));
#7384=DIRECTION('',(-0.948122329809732,-5.77180576401594E-5,-0.317905716187664));
#7385=DIRECTION('',(0.317905711303626,8.02290542263056E-5,-0.948122329809732));
#7386=DIRECTION('',(-0.948122329809733,-5.77180576406142E-5,-0.317905716187663));
#7387=DIRECTION('',(0.317905711303625,8.02290542261712E-5,-0.948122329809732));
#7388=CARTESIAN_POINT('',(0.,0.,0.));
#7389=CARTESIAN_POINT('',(0.,0.,0.));
#7390=CARTESIAN_POINT('Origin',(-0.0735499999997847,-0.0149749999999933,
0.02565));
#7391=CARTESIAN_POINT('',(-0.0735499999997877,-0.0171999999999932,0.053125));
#7392=CARTESIAN_POINT('',(-0.0735499999997876,-0.0171999999999933,0.061125));
#7393=CARTESIAN_POINT('',(-0.0735499999997877,-0.0171999999999932,0.053125));
#7394=CARTESIAN_POINT('',(-0.0735499999997809,-0.0121999999999932,0.066125));
#7395=CARTESIAN_POINT('Origin',(-0.0735499999997809,-0.0121999999999932,
0.061125));
#7396=CARTESIAN_POINT('',(-0.073549999999775,-0.00774999999999323,0.066125));
#7397=CARTESIAN_POINT('',(-0.0735499999997809,-0.0121999999999932,0.066125));
#7398=CARTESIAN_POINT('',(-0.0735499999997682,-0.00274999999999323,0.061125));
#7399=CARTESIAN_POINT('Origin',(-0.073549999999775,-0.00774999999999327,
0.061125));
#7400=CARTESIAN_POINT('',(-0.0735499999997682,-0.00274999999999327,-0.009825));
#7401=CARTESIAN_POINT('',(-0.0735499999997682,-0.00274999999999323,0.061125));
#7402=CARTESIAN_POINT('',(-0.0735499999997749,-0.0077499999999933,-0.014825));
#7403=CARTESIAN_POINT('Origin',(-0.0735499999997749,-0.0077499999999933,
-0.00982499999999996));
#7404=CARTESIAN_POINT('',(-0.0735499999997809,-0.0121999999999933,-0.014825));
#7405=CARTESIAN_POINT('',(-0.0735499999997749,-0.0077499999999933,-0.014825));
#7406=CARTESIAN_POINT('',(-0.0735499999997876,-0.0171999999999933,-0.00982499999999996));
#7407=CARTESIAN_POINT('Origin',(-0.0735499999997809,-0.0121999999999933,
-0.00982499999999996));
#7408=CARTESIAN_POINT('',(-0.0735499999997877,-0.0171999999999932,-0.00182499999999996));
#7409=CARTESIAN_POINT('',(-0.0735499999997876,-0.0171999999999933,-0.00982499999999996));
#7410=CARTESIAN_POINT('',(-0.0735499999997944,-0.0221999999999932,0.00317500000000004));
#7411=CARTESIAN_POINT('Origin',(-0.0735499999997944,-0.0221999999999932,
-0.00182499999999997));
#7412=CARTESIAN_POINT('',(-0.0735499999998011,-0.0271999999999932,0.00817500000000003));
#7413=CARTESIAN_POINT('Origin',(-0.0735499999997944,-0.0221999999999932,
0.00817500000000003));
#7414=CARTESIAN_POINT('',(-0.0735499999998011,-0.0271999999999932,0.043125));
#7415=CARTESIAN_POINT('',(-0.0735499999998011,-0.0271999999999932,0.00817500000000003));
#7416=CARTESIAN_POINT('',(-0.0735499999997944,-0.0221999999999932,0.0481250000000001));
#7417=CARTESIAN_POINT('Origin',(-0.0735499999997944,-0.0221999999999932,
0.043125));
#7418=CARTESIAN_POINT('Origin',(-0.0735499999997944,-0.0221999999999932,
0.0531250000000001));
#7419=CARTESIAN_POINT('Origin',(-0.06655,-0.0172,0.02565));
#7420=CARTESIAN_POINT('',(-0.04655,-0.0172,-0.001825));
#7421=CARTESIAN_POINT('',(-0.04655,-0.0172,-0.009825));
#7422=CARTESIAN_POINT('',(-0.04655,-0.0172,0.02565));
#7423=CARTESIAN_POINT('',(-0.06655,-0.0172,-0.001825));
#7424=CARTESIAN_POINT('',(-0.04655,-0.0172,-0.009825));
#7425=CARTESIAN_POINT('Origin',(-0.06655,-0.009975,0.066125));
#7426=CARTESIAN_POINT('',(-0.04655,-0.0122,0.066125));
#7427=CARTESIAN_POINT('',(-0.06655,-0.0122,0.066125));
#7428=CARTESIAN_POINT('',(-0.04655,-0.00775,0.066125));
#7429=CARTESIAN_POINT('',(-0.04655,-0.009975,0.066125));
#7430=CARTESIAN_POINT('',(-0.068549999999775,-0.00774999999999995,0.066125));
#7431=CARTESIAN_POINT('Origin',(-0.06655,-0.00275,0.02565));
#7432=CARTESIAN_POINT('',(-0.04655,-0.00275,0.061125));
#7433=CARTESIAN_POINT('',(-0.04655,-0.00275,0.061125));
#7434=CARTESIAN_POINT('',(-0.04655,-0.00275,-0.009825));
#7435=CARTESIAN_POINT('',(-0.04655,-0.00275,0.02565));
#7436=CARTESIAN_POINT('',(-0.0685499999997682,-0.00274999999999999,-0.009825));
#7437=CARTESIAN_POINT('',(-0.05755,-0.00275,0.0218));
#7438=CARTESIAN_POINT('Origin',(-0.05755,-0.00275,0.014175));
#7439=CARTESIAN_POINT('',(-0.05755,-0.00275,0.04475));
#7440=CARTESIAN_POINT('Origin',(-0.05755,-0.00275,0.037125));
#7441=CARTESIAN_POINT('Origin',(-0.06655,-0.009975,-0.014825));
#7442=CARTESIAN_POINT('',(-0.04655,-0.00775,-0.014825));
#7443=CARTESIAN_POINT('',(-0.06655,-0.00775,-0.014825));
#7444=CARTESIAN_POINT('',(-0.04655,-0.0122,-0.014825));
#7445=CARTESIAN_POINT('',(-0.04655,-0.009975,-0.014825));
#7446=CARTESIAN_POINT('',(-0.0685499999997809,-0.0122,-0.014825));
#7447=CARTESIAN_POINT('Origin',(-0.06655,-0.009975,-0.0076));
#7448=CARTESIAN_POINT('',(-0.06655,-0.009975,-0.003375));
#7449=CARTESIAN_POINT('Origin',(-0.06655,-0.009975,-0.0076));
#7450=CARTESIAN_POINT('',(-0.04655,-0.009975,-0.003375));
#7451=CARTESIAN_POINT('',(-0.06655,-0.009975,-0.003375));
#7452=CARTESIAN_POINT('Origin',(-0.04655,-0.009975,-0.0076));
#7453=CARTESIAN_POINT('Origin',(-0.06655,-0.0172,0.02565));
#7454=CARTESIAN_POINT('',(-0.04655,-0.0172,0.053125));
#7455=CARTESIAN_POINT('',(-0.04655,-0.0172,0.053125));
#7456=CARTESIAN_POINT('',(-0.04655,-0.0172,0.061125));
#7457=CARTESIAN_POINT('',(-0.04655,-0.0172,0.02565));
#7458=CARTESIAN_POINT('',(-0.0685499999997877,-0.0172,0.061125));
#7459=CARTESIAN_POINT('Origin',(-0.06655,-0.01,0.0589));
#7460=CARTESIAN_POINT('',(-0.06655,-0.01,0.063125));
#7461=CARTESIAN_POINT('Origin',(-0.06655,-0.01,0.0589));
#7462=CARTESIAN_POINT('',(-0.04655,-0.01,0.063125));
#7463=CARTESIAN_POINT('',(-0.06655,-0.01,0.063125));
#7464=CARTESIAN_POINT('Origin',(-0.04655,-0.01,0.0589));
#7465=CARTESIAN_POINT('Origin',(-0.04655,0.,0.02565));
#7466=CARTESIAN_POINT('',(-0.04655,-0.0272,0.043125));
#7467=CARTESIAN_POINT('',(-0.04655,-0.0272,0.008175));
#7468=CARTESIAN_POINT('',(-0.04655,-0.0272,0.02565));
#7469=CARTESIAN_POINT('',(-0.04655,-0.0222,0.003175));
#7470=CARTESIAN_POINT('Origin',(-0.04655,-0.0222,0.008175));
#7471=CARTESIAN_POINT('Origin',(-0.04655,-0.0222,-0.001825));
#7472=CARTESIAN_POINT('Origin',(-0.04655,-0.0122,-0.009825));
#7473=CARTESIAN_POINT('Origin',(-0.04655,-0.00775,-0.009825));
#7474=CARTESIAN_POINT('Origin',(-0.04655,-0.00775,0.061125));
#7475=CARTESIAN_POINT('Origin',(-0.04655,-0.0122,0.061125));
#7476=CARTESIAN_POINT('',(-0.04655,-0.0222,0.048125));
#7477=CARTESIAN_POINT('Origin',(-0.04655,-0.0222,0.053125));
#7478=CARTESIAN_POINT('Origin',(-0.04655,-0.0222,0.043125));
#7479=CARTESIAN_POINT('Origin',(-0.06655,-0.009975,0.02565));
#7480=CARTESIAN_POINT('Origin',(-0.06655,-0.009975,0.02565));
#7481=CARTESIAN_POINT('Origin',(-0.06655,-0.0122,0.061125));
#7482=CARTESIAN_POINT('Origin',(-0.06655,-0.00775,0.061125));
#7483=CARTESIAN_POINT('Origin',(-0.06655,-0.00775,-0.009825));
#7484=CARTESIAN_POINT('Origin',(-0.06655,-0.0122,-0.009825));
#7485=CARTESIAN_POINT('Origin',(-0.05755,-0.0272,0.02565));
#7486=CARTESIAN_POINT('',(-0.0622553825561797,-0.0272,0.008175));
#7487=CARTESIAN_POINT('',(-0.0685499999998011,-0.0271999999999999,0.00817500000000003));
#7488=CARTESIAN_POINT('',(-0.05755,-0.0272,0.0218));
#7489=CARTESIAN_POINT('Origin',(-0.05755,-0.0272,0.014175));
#7490=CARTESIAN_POINT('',(-0.0528446174438203,-0.0272,0.008175));
#7491=CARTESIAN_POINT('Origin',(-0.05755,-0.0272,0.014175));
#7492=CARTESIAN_POINT('',(-0.04655,-0.0272,0.008175));
#7493=CARTESIAN_POINT('',(-0.0528446174438203,-0.0272,0.043125));
#7494=CARTESIAN_POINT('',(-0.05755,-0.0272,0.043125));
#7495=CARTESIAN_POINT('',(-0.0622553825561797,-0.0272,0.043125));
#7496=CARTESIAN_POINT('Origin',(-0.05755,-0.0272,0.037125));
#7497=CARTESIAN_POINT('',(-0.0685499999998011,-0.0272,0.043125));
#7498=CARTESIAN_POINT('Origin',(-0.05755,-0.0022,0.037125));
#7499=CARTESIAN_POINT('',(-0.05755,-0.0269285700798444,0.04475));
#7500=CARTESIAN_POINT('',(-0.05755,-0.0022,0.04475));
#7501=CARTESIAN_POINT('Ctrl Pts',(-0.0622553825561797,-0.0272,0.043125));
#7502=CARTESIAN_POINT('Ctrl Pts',(-0.0617185912965407,-0.0272,0.0435459680382359));
#7503=CARTESIAN_POINT('Ctrl Pts',(-0.0611100942808263,-0.027146490983882,
0.0439040351600042));
#7504=CARTESIAN_POINT('Ctrl Pts',(-0.0595292759370733,-0.0270066019492738,
0.0445577665669935));
#7505=CARTESIAN_POINT('Ctrl Pts',(-0.058511387005684,-0.0269285700798444,
0.04475));
#7506=CARTESIAN_POINT('Ctrl Pts',(-0.05755,-0.0269285700798444,0.04475));
#7507=CARTESIAN_POINT('Ctrl Pts',(-0.05755,-0.0269285700798444,0.04475));
#7508=CARTESIAN_POINT('Ctrl Pts',(-0.056588612994316,-0.0269285700798444,
0.04475));
#7509=CARTESIAN_POINT('Ctrl Pts',(-0.0555707240629267,-0.0270066019492738,
0.0445577665669935));
#7510=CARTESIAN_POINT('Ctrl Pts',(-0.0539899057191737,-0.027146490983882,
0.0439040351600042));
#7511=CARTESIAN_POINT('Ctrl Pts',(-0.0533814087034593,-0.0272,0.0435459680382359));
#7512=CARTESIAN_POINT('Ctrl Pts',(-0.0528446174438203,-0.0272,0.043125));
#7513=CARTESIAN_POINT('Origin',(-0.05755,-0.0022,0.014175));
#7514=CARTESIAN_POINT('',(-0.05755,-0.0022,0.0218));
#7515=CARTESIAN_POINT('Ctrl Pts',(-0.0622553825561797,-0.0272,0.00817500000000001));
#7516=CARTESIAN_POINT('Ctrl Pts',(-0.0617185912965407,-0.0272,0.00775403196176415));
#7517=CARTESIAN_POINT('Ctrl Pts',(-0.0611100942808263,-0.027146490983882,
0.00739596483999584));
#7518=CARTESIAN_POINT('Ctrl Pts',(-0.0595292759370733,-0.0270066019492738,
0.00674223343300649));
#7519=CARTESIAN_POINT('Ctrl Pts',(-0.058511387005684,-0.0269285700798444,
0.00655));
#7520=CARTESIAN_POINT('Ctrl Pts',(-0.056588612994316,-0.0269285700798444,
0.00655));
#7521=CARTESIAN_POINT('Ctrl Pts',(-0.0555707240629267,-0.0270066019492738,
0.00674223343300649));
#7522=CARTESIAN_POINT('Ctrl Pts',(-0.0539899057191737,-0.027146490983882,
0.00739596483999584));
#7523=CARTESIAN_POINT('Ctrl Pts',(-0.0533814087034593,-0.0272,0.00775403196176415));
#7524=CARTESIAN_POINT('Ctrl Pts',(-0.0528446174438203,-0.0272,0.00817500000000001));
#7525=CARTESIAN_POINT('Origin',(-0.05755,-0.0222,0.008175));
#7526=CARTESIAN_POINT('',(-0.0685499999997944,-0.0221999999999999,0.00317500000000004));
#7527=CARTESIAN_POINT('Origin',(-0.05755,-0.0222,-0.001825));
#7528=CARTESIAN_POINT('Origin',(-0.05755,-0.0222,0.043125));
#7529=CARTESIAN_POINT('',(-0.0685499999997944,-0.0221999999999999,0.0481250000000001));
#7530=CARTESIAN_POINT('Origin',(-0.06655,-0.0222,0.053125));
#7531=CARTESIAN_POINT('',(0.,0.,0.));
#7532=CARTESIAN_POINT('Origin',(0.0232500000002624,0.0199999999999376,0.0120000000000001));
#7533=CARTESIAN_POINT('',(0.02175,0.00499999999993959,0.012));
#7534=CARTESIAN_POINT('',(0.02175,0.0199999999999396,0.0120000000000001));
#7535=CARTESIAN_POINT('',(0.02175,0.0104999999999688,0.0120000000000001));
#7536=CARTESIAN_POINT('',(0.0232500000002423,0.00499999999993758,0.012));
#7537=CARTESIAN_POINT('',(0.0232500000002423,0.00499999999993758,0.012));
#7538=CARTESIAN_POINT('',(0.0232500000002624,0.0199999999999376,0.0120000000000001));
#7539=CARTESIAN_POINT('',(0.02325,0.00999999999996881,0.0120000000000001));
#7540=CARTESIAN_POINT('',(0.0116250000001312,0.02,0.0120000000000001));
#7541=CARTESIAN_POINT('Origin',(0.0232500000002422,0.00499999999993754,
0.032));
#7542=CARTESIAN_POINT('',(0.02175,0.0199999999999396,0.0320000000000001));
#7543=CARTESIAN_POINT('',(0.02175,0.00499999999993952,0.032));
#7544=CARTESIAN_POINT('',(0.02175,0.00299999999996879,0.032));
#7545=CARTESIAN_POINT('',(0.0232500000002624,0.0199999999999376,0.0320000000000001));
#7546=CARTESIAN_POINT('',(0.0116250000001211,0.02,0.0320000000000001));
#7547=CARTESIAN_POINT('',(0.0232500000002422,0.00499999999993751,0.032));
#7548=CARTESIAN_POINT('',(0.02325,0.00249999999996874,0.032));
#7549=CARTESIAN_POINT('',(0.0232500000002422,0.00499999999993751,0.032));
#7550=CARTESIAN_POINT('Origin',(0.0232500000002423,0.00499999999993758,
0.012));
#7551=CARTESIAN_POINT('',(0.02175,0.00499999999993956,0.029));
#7552=CARTESIAN_POINT('',(0.02325,0.00499999999993759,0.00700000000000003));
#7553=CARTESIAN_POINT('Origin',(0.,0.02,0.002));
#7554=CARTESIAN_POINT('',(0.02325,0.02,0.));
#7555=CARTESIAN_POINT('',(0.02325,0.02,0.002));
#7556=CARTESIAN_POINT('',(-0.02325,0.02,0.));
#7557=CARTESIAN_POINT('',(0.,0.02,0.));
#7558=CARTESIAN_POINT('',(-0.02325,0.02,0.012));
#7559=CARTESIAN_POINT('',(-0.02325,0.02,0.002));
#7560=CARTESIAN_POINT('',(-0.02175,0.02,0.012));
#7561=CARTESIAN_POINT('',(-0.01325,0.02,0.012));
#7562=CARTESIAN_POINT('',(-0.02175,0.02,0.002));
#7563=CARTESIAN_POINT('',(-0.02175,0.02,0.046));
#7564=CARTESIAN_POINT('',(0.02175,0.02,0.002));
#7565=CARTESIAN_POINT('',(0.,0.02,0.002));
#7566=CARTESIAN_POINT('',(0.02175,0.02,0.046));
#7567=CARTESIAN_POINT('Origin',(0.,0.02,0.002));
#7568=CARTESIAN_POINT('',(0.02175,0.02,0.046));
#7569=CARTESIAN_POINT('',(0.02175,0.02,0.046));
#7570=CARTESIAN_POINT('',(-0.02175,0.02,0.046));
#7571=CARTESIAN_POINT('',(0.,0.02,0.046));
#7572=CARTESIAN_POINT('',(-0.02175,0.02,0.032));
#7573=CARTESIAN_POINT('',(-0.02175,0.02,0.046));
#7574=CARTESIAN_POINT('',(-0.02325,0.02,0.032));
#7575=CARTESIAN_POINT('',(-0.01325,0.02,0.032));
#7576=CARTESIAN_POINT('',(-0.02325,0.02,0.051));
#7577=CARTESIAN_POINT('',(-0.02325,0.02,0.002));
#7578=CARTESIAN_POINT('',(0.02325,0.02,0.051));
#7579=CARTESIAN_POINT('',(0.,0.02,0.051));
#7580=CARTESIAN_POINT('',(0.02325,0.02,0.002));
#7581=CARTESIAN_POINT('Origin',(0.02175,0.001,0.046));
#7582=CARTESIAN_POINT('',(0.02175,-0.018,0.002));
#7583=CARTESIAN_POINT('',(0.02175,0.001,0.002));
#7584=CARTESIAN_POINT('',(0.02175,-0.018,0.046));
#7585=CARTESIAN_POINT('',(0.02175,-0.018,0.046));
#7586=CARTESIAN_POINT('',(0.02175,0.001,0.046));
#7587=CARTESIAN_POINT('Origin',(0.0232500000002423,0.00500000000000003,
0.0560000000000001));
#7588=CARTESIAN_POINT('',(-0.02325,0.005,0.051));
#7589=CARTESIAN_POINT('',(-0.02325,0.00500000000006252,0.0560000000000001));
#7590=CARTESIAN_POINT('',(-0.02325,0.0050000000000625,0.0547500000000001));
#7591=CARTESIAN_POINT('',(0.0232500000002422,0.00500000000000004,0.0560000000000001));
#7592=CARTESIAN_POINT('',(1.24499124710741E-13,0.00500000000003127,0.0560000000000001));
#7593=CARTESIAN_POINT('',(0.02325,0.005,0.051));
#7594=CARTESIAN_POINT('',(0.0232500000002423,0.005,0.0510000000000001));
#7595=CARTESIAN_POINT('',(0.02325,0.005,0.051));
#7596=CARTESIAN_POINT('Origin',(-0.0232499999999731,0.0199999999998699,
0.0560000000000001));
#7597=CARTESIAN_POINT('',(-0.0232499999999731,0.0199999999998699,0.0560000000000001));
#7598=CARTESIAN_POINT('',(-0.0232499999999731,0.0199999999998699,0.0560000000000001));
#7599=CARTESIAN_POINT('',(0.0232500000000269,0.0199999999998074,0.0560000000000001));
#7600=CARTESIAN_POINT('',(0.0232500000000269,0.0199999999998074,0.0560000000000001));
#7601=CARTESIAN_POINT('',(0.0232500000000269,0.0199999999998074,0.0560000000000001));
#7602=CARTESIAN_POINT('Origin',(2.69118061169138E-14,0.0199999999998387,
0.0585000000000001));
#7603=CARTESIAN_POINT('',(-0.0232499999999731,0.0199999999998699,0.0610000000000001));
#7604=CARTESIAN_POINT('',(0.0232500000000269,0.0199999999998075,0.0610000000000001));
#7605=CARTESIAN_POINT('',(-0.0232499999999731,0.0199999999998699,0.0610000000000001));
#7606=CARTESIAN_POINT('',(0.0232500000000269,0.0199999999998075,0.0610000000000001));
#7607=CARTESIAN_POINT('',(-0.0232499999999731,0.0199999999998699,0.0560000000000001));
#7608=CARTESIAN_POINT('Origin',(0.,0.,0.046));
#7609=CARTESIAN_POINT('',(-0.02175,-0.018,0.046));
#7610=CARTESIAN_POINT('',(-0.02175,0.001,0.046));
#7611=CARTESIAN_POINT('',(6.93889390390723E-18,-0.018,0.046));
#7612=CARTESIAN_POINT('',(-0.01825,-0.0127,0.046));
#7613=CARTESIAN_POINT('',(-0.01825,-0.0175,0.046));
#7614=CARTESIAN_POINT('',(-0.01825,-0.01625,0.046));
#7615=CARTESIAN_POINT('',(-0.02125,-0.0127,0.046));
#7616=CARTESIAN_POINT('',(0.,-0.0127,0.046));
#7617=CARTESIAN_POINT('',(-0.02125,-0.0175,0.046));
#7618=CARTESIAN_POINT('',(-0.02125,-0.01625,0.046));
#7619=CARTESIAN_POINT('',(-0.01975,-0.0175,0.046));
#7620=CARTESIAN_POINT('',(0.00525,-0.0127,0.046));
#7621=CARTESIAN_POINT('',(0.00525,-0.0175,0.046));
#7622=CARTESIAN_POINT('',(0.00525,-0.01625,0.046));
#7623=CARTESIAN_POINT('',(0.00225,-0.0127,0.046));
#7624=CARTESIAN_POINT('',(7.3436627149685E-18,-0.0127,0.046));
#7625=CARTESIAN_POINT('',(0.00225,-0.0175,0.046));
#7626=CARTESIAN_POINT('',(0.00225,-0.01625,0.046));
#7627=CARTESIAN_POINT('',(0.00375,-0.0175,0.046));
#7628=CARTESIAN_POINT('',(0.01825,-0.0073,0.046));
#7629=CARTESIAN_POINT('',(0.02125,-0.0073,0.046));
#7630=CARTESIAN_POINT('',(0.02125,-0.0073,0.046));
#7631=CARTESIAN_POINT('',(0.02125,-0.0025,0.046));
#7632=CARTESIAN_POINT('',(0.02125,-0.00375,0.046));
#7633=CARTESIAN_POINT('',(0.01825,-0.0025,0.046));
#7634=CARTESIAN_POINT('',(0.01975,-0.0025,0.046));
#7635=CARTESIAN_POINT('',(0.01825,-0.00375,0.046));
#7636=CARTESIAN_POINT('',(-0.00525,-0.0073,0.046));
#7637=CARTESIAN_POINT('',(-0.00225,-0.0073,0.046));
#7638=CARTESIAN_POINT('',(-0.00225,-0.0073,0.046));
#7639=CARTESIAN_POINT('',(-0.00225,-0.0025,0.046));
#7640=CARTESIAN_POINT('',(-0.00225,-0.00375,0.046));
#7641=CARTESIAN_POINT('',(-0.00525,-0.0025,0.046));
#7642=CARTESIAN_POINT('',(-0.00375,-0.0025,0.046));
#7643=CARTESIAN_POINT('',(-0.00525,-0.00375,0.046));
#7644=CARTESIAN_POINT('',(0.00225,-0.0073,0.046));
#7645=CARTESIAN_POINT('',(0.00525,-0.0073,0.046));
#7646=CARTESIAN_POINT('',(0.00525,-0.0073,0.046));
#7647=CARTESIAN_POINT('',(0.00525,-0.0025,0.046));
#7648=CARTESIAN_POINT('',(0.00525,-0.00375,0.046));
#7649=CARTESIAN_POINT('',(0.00225,-0.0025,0.046));
#7650=CARTESIAN_POINT('',(0.00375,-0.0025,0.046));
#7651=CARTESIAN_POINT('',(0.00225,-0.00375,0.046));
#7652=CARTESIAN_POINT('',(0.02125,-0.0127,0.046));
#7653=CARTESIAN_POINT('',(0.02125,-0.0175,0.046));
#7654=CARTESIAN_POINT('',(0.02125,-0.01625,0.046));
#7655=CARTESIAN_POINT('',(0.01825,-0.0127,0.046));
#7656=CARTESIAN_POINT('',(0.,-0.0127,0.046));
#7657=CARTESIAN_POINT('',(0.01825,-0.0175,0.046));
#7658=CARTESIAN_POINT('',(0.01825,-0.01625,0.046));
#7659=CARTESIAN_POINT('',(0.01975,-0.0175,0.046));
#7660=CARTESIAN_POINT('',(-0.00225,-0.0127,0.046));
#7661=CARTESIAN_POINT('',(-0.00525,-0.0127,0.046));
#7662=CARTESIAN_POINT('',(-0.00525,-0.0127,0.046));
#7663=CARTESIAN_POINT('',(-0.00525,-0.0175,0.046));
#7664=CARTESIAN_POINT('',(-0.00525,-0.01625,0.046));
#7665=CARTESIAN_POINT('',(-0.00225,-0.0175,0.046));
#7666=CARTESIAN_POINT('',(-0.00375,-0.0175,0.046));
#7667=CARTESIAN_POINT('',(-0.00225,-0.01625,0.046));
#7668=CARTESIAN_POINT('',(-0.02125,-0.0073,0.046));
#7669=CARTESIAN_POINT('',(-0.01825,-0.0073,0.046));
#7670=CARTESIAN_POINT('',(-0.01825,-0.0073,0.046));
#7671=CARTESIAN_POINT('',(-0.01825,-0.0025,0.046));
#7672=CARTESIAN_POINT('',(-0.01825,-0.00375,0.046));
#7673=CARTESIAN_POINT('',(-0.02125,-0.0025,0.046));
#7674=CARTESIAN_POINT('',(-0.01975,-0.0025,0.046));
#7675=CARTESIAN_POINT('',(-0.02125,-0.00375,0.046));
#7676=CARTESIAN_POINT('Origin',(0.01825,-0.01625,0.061));
#7677=CARTESIAN_POINT('',(0.01825,-0.017211102550928,0.061));
#7678=CARTESIAN_POINT('',(0.01825,-0.0175,0.0598288205727445));
#7679=CARTESIAN_POINT('Origin',(0.01825,-0.01,0.0586));
#7680=CARTESIAN_POINT('',(0.01825,-0.0175,0.061));
#7681=CARTESIAN_POINT('',(0.01825,-0.01625,0.061));
#7682=CARTESIAN_POINT('',(0.01825,-0.0175,0.061));
#7683=CARTESIAN_POINT('Origin',(0.02125,-0.01625,0.061));
#7684=CARTESIAN_POINT('',(0.02125,-0.017211102550928,0.061));
#7685=CARTESIAN_POINT('',(0.02125,-0.0175,0.061));
#7686=CARTESIAN_POINT('',(0.02125,-0.01625,0.061));
#7687=CARTESIAN_POINT('',(0.02125,-0.0175,0.0598288205727445));
#7688=CARTESIAN_POINT('Origin',(0.02125,-0.01,0.0586));
#7689=CARTESIAN_POINT('',(0.02125,-0.0175,0.061));
#7690=CARTESIAN_POINT('Origin',(0.00225,-0.01625,0.061));
#7691=CARTESIAN_POINT('',(0.00225,-0.017211102550928,0.061));
#7692=CARTESIAN_POINT('',(0.00225,-0.0175,0.0598288205727445));
#7693=CARTESIAN_POINT('Origin',(0.00225,-0.01,0.0586));
#7694=CARTESIAN_POINT('',(0.00225,-0.0175,0.061));
#7695=CARTESIAN_POINT('',(0.00225,-0.01625,0.061));
#7696=CARTESIAN_POINT('',(0.00225,-0.0175,0.061));
#7697=CARTESIAN_POINT('Origin',(0.00525,-0.01625,0.061));
#7698=CARTESIAN_POINT('',(0.00525,-0.017211102550928,0.061));
#7699=CARTESIAN_POINT('',(0.00525,-0.0175,0.061));
#7700=CARTESIAN_POINT('',(0.00525,-0.01625,0.061));
#7701=CARTESIAN_POINT('',(0.00525,-0.0175,0.0598288205727445));
#7702=CARTESIAN_POINT('Origin',(0.00525,-0.01,0.0586));
#7703=CARTESIAN_POINT('',(0.00525,-0.0175,0.061));
#7704=CARTESIAN_POINT('Origin',(0.00225,-0.00375,0.061));
#7705=CARTESIAN_POINT('',(0.00225,-0.0025,0.0598288205727444));
#7706=CARTESIAN_POINT('',(0.00225,-0.00278889744907202,0.061));
#7707=CARTESIAN_POINT('Origin',(0.00225,-0.01,0.0586));
#7708=CARTESIAN_POINT('',(0.00225,-0.0025,0.061));
#7709=CARTESIAN_POINT('',(0.00225,-0.0025,0.061));
#7710=CARTESIAN_POINT('',(0.00225,-0.00375,0.061));
#7711=CARTESIAN_POINT('Origin',(-0.00225,-0.01625,0.061));
#7712=CARTESIAN_POINT('',(-0.00225,-0.0175,0.0598288205727445));
#7713=CARTESIAN_POINT('',(-0.00225,-0.017211102550928,0.061));
#7714=CARTESIAN_POINT('Origin',(-0.00225,-0.01,0.0586));
#7715=CARTESIAN_POINT('',(-0.00225,-0.0175,0.061));
#7716=CARTESIAN_POINT('',(-0.00225,-0.0175,0.061));
#7717=CARTESIAN_POINT('',(-0.00225,-0.01625,0.061));
#7718=CARTESIAN_POINT('Origin',(-0.00375,-0.0175,0.061));
#7719=CARTESIAN_POINT('',(-0.00525,-0.0175,0.0598288205727445));
#7720=CARTESIAN_POINT('',(0.02675,-0.0175,0.0598288205727445));
#7721=CARTESIAN_POINT('',(-0.00525,-0.0175,0.061));
#7722=CARTESIAN_POINT('',(-0.00525,-0.0175,0.061));
#7723=CARTESIAN_POINT('',(-0.00375,-0.0175,0.061));
#7724=CARTESIAN_POINT('Origin',(-0.00225,-0.00375,0.061));
#7725=CARTESIAN_POINT('',(-0.00225,-0.0025,0.061));
#7726=CARTESIAN_POINT('',(-0.00225,-0.0025,0.0598288205727444));
#7727=CARTESIAN_POINT('',(-0.00225,-0.0025,0.061));
#7728=CARTESIAN_POINT('',(-0.00225,-0.00278889744907202,0.061));
#7729=CARTESIAN_POINT('Origin',(-0.00225,-0.01,0.0586));
#7730=CARTESIAN_POINT('',(-0.00225,-0.00375,0.061));
#7731=CARTESIAN_POINT('Origin',(-0.02125,-0.01625,0.061));
#7732=CARTESIAN_POINT('',(-0.02125,-0.017211102550928,0.061));
#7733=CARTESIAN_POINT('',(-0.02125,-0.0175,0.0598288205727445));
#7734=CARTESIAN_POINT('Origin',(-0.02125,-0.01,0.0586));
#7735=CARTESIAN_POINT('',(-0.02125,-0.0175,0.061));
#7736=CARTESIAN_POINT('',(-0.02125,-0.01625,0.061));
#7737=CARTESIAN_POINT('',(-0.02125,-0.0175,0.061));
#7738=CARTESIAN_POINT('Origin',(-0.01825,-0.01625,0.061));
#7739=CARTESIAN_POINT('',(-0.01825,-0.017211102550928,0.061));
#7740=CARTESIAN_POINT('',(-0.01825,-0.0175,0.061));
#7741=CARTESIAN_POINT('',(-0.01825,-0.01625,0.061));
#7742=CARTESIAN_POINT('',(-0.01825,-0.0175,0.0598288205727445));
#7743=CARTESIAN_POINT('Origin',(-0.01825,-0.01,0.0586));
#7744=CARTESIAN_POINT('',(-0.01825,-0.0175,0.061));
#7745=CARTESIAN_POINT('Origin',(-3.46944695195361E-18,0.,0.061));
#7746=CARTESIAN_POINT('',(0.02325,-0.017211102550928,0.061));
#7747=CARTESIAN_POINT('',(0.02325,-0.02,0.061));
#7748=CARTESIAN_POINT('',(0.02325,3.46944695195361E-18,0.061));
#7749=CARTESIAN_POINT('',(0.02675,-0.017211102550928,0.061));
#7750=CARTESIAN_POINT('',(0.01975,-0.0175,0.061));
#7751=CARTESIAN_POINT('',(0.02675,-0.017211102550928,0.061));
#7752=CARTESIAN_POINT('',(0.00375,-0.0175,0.061));
#7753=CARTESIAN_POINT('',(0.02675,-0.017211102550928,0.061));
#7754=CARTESIAN_POINT('',(-0.00525,-0.017211102550928,0.061));
#7755=CARTESIAN_POINT('',(-0.00525,-0.01625,0.061));
#7756=CARTESIAN_POINT('',(0.02675,-0.017211102550928,0.061));
#7757=CARTESIAN_POINT('',(-0.01975,-0.0175,0.061));
#7758=CARTESIAN_POINT('',(-0.02325,-0.017211102550928,0.061));
#7759=CARTESIAN_POINT('',(0.02675,-0.017211102550928,0.061));
#7760=CARTESIAN_POINT('',(-0.02325,-0.02,0.061));
#7761=CARTESIAN_POINT('',(-0.02325,-3.46944695195361E-18,0.061));
#7762=CARTESIAN_POINT('',(0.,-0.02,0.061));
#7763=CARTESIAN_POINT('Origin',(0.,0.,0.051));
#7764=CARTESIAN_POINT('',(-0.02325,-3.46944695195361E-18,0.051));
#7765=CARTESIAN_POINT('',(0.02325,3.46944695195361E-18,0.051));
#7766=CARTESIAN_POINT('Origin',(0.,0.,0.002));
#7767=CARTESIAN_POINT('',(-0.02175,-0.018,0.002));
#7768=CARTESIAN_POINT('',(-0.02175,0.001,0.002));
#7769=CARTESIAN_POINT('',(6.93889390390723E-18,-0.018,0.002));
#7770=CARTESIAN_POINT('',(-0.02125,-0.0127,0.002));
#7771=CARTESIAN_POINT('',(-0.02125,-0.0175,0.002));
#7772=CARTESIAN_POINT('',(-0.02125,0.,0.002));
#7773=CARTESIAN_POINT('',(-0.01825,-0.0127,0.002));
#7774=CARTESIAN_POINT('',(0.,-0.0127,0.002));
#7775=CARTESIAN_POINT('',(-0.01825,-0.0175,0.002));
#7776=CARTESIAN_POINT('',(-0.01825,0.,0.002));
#7777=CARTESIAN_POINT('',(0.,-0.0175,0.002));
#7778=CARTESIAN_POINT('',(-0.01825,-0.0073,0.002));
#7779=CARTESIAN_POINT('',(-0.02125,-0.0073,0.002));
#7780=CARTESIAN_POINT('',(-0.02125,-0.0073,0.002));
#7781=CARTESIAN_POINT('',(-0.02125,-0.0025,0.002));
#7782=CARTESIAN_POINT('',(-0.02125,0.,0.002));
#7783=CARTESIAN_POINT('',(-0.01825,-0.0025,0.002));
#7784=CARTESIAN_POINT('',(0.,-0.0025,0.002));
#7785=CARTESIAN_POINT('',(-0.01825,0.,0.002));
#7786=CARTESIAN_POINT('',(-0.00225,-0.0073,0.002));
#7787=CARTESIAN_POINT('',(-0.00225,-0.0025,0.002));
#7788=CARTESIAN_POINT('',(-0.00225,3.90312782094781E-19,0.002));
#7789=CARTESIAN_POINT('',(-0.00525,-0.0073,0.002));
#7790=CARTESIAN_POINT('',(-2.11058022910511E-18,-0.0073,0.002));
#7791=CARTESIAN_POINT('',(-0.00525,-0.0025,0.002));
#7792=CARTESIAN_POINT('',(-0.00525,0.,0.002));
#7793=CARTESIAN_POINT('',(-3.61400724161836E-19,-0.0025,0.002));
#7794=CARTESIAN_POINT('',(0.00525,-0.0073,0.002));
#7795=CARTESIAN_POINT('',(0.00225,-0.0073,0.002));
#7796=CARTESIAN_POINT('',(0.00225,-0.0073,0.002));
#7797=CARTESIAN_POINT('',(0.00225,-0.0025,0.002));
#7798=CARTESIAN_POINT('',(0.00225,-3.90312782094781E-19,0.002));
#7799=CARTESIAN_POINT('',(0.00525,-0.0025,0.002));
#7800=CARTESIAN_POINT('',(-7.2280144832367E-19,-0.0025,0.002));
#7801=CARTESIAN_POINT('',(0.00525,0.,0.002));
#7802=CARTESIAN_POINT('',(0.02125,-0.0073,0.002));
#7803=CARTESIAN_POINT('',(0.01825,-0.0073,0.002));
#7804=CARTESIAN_POINT('',(0.01825,-0.0073,0.002));
#7805=CARTESIAN_POINT('',(0.01825,-0.0025,0.002));
#7806=CARTESIAN_POINT('',(0.01825,0.,0.002));
#7807=CARTESIAN_POINT('',(0.02125,-0.0025,0.002));
#7808=CARTESIAN_POINT('',(0.,-0.0025,0.002));
#7809=CARTESIAN_POINT('',(0.02125,0.,0.002));
#7810=CARTESIAN_POINT('',(0.01825,-0.0127,0.002));
#7811=CARTESIAN_POINT('',(0.01825,-0.0175,0.002));
#7812=CARTESIAN_POINT('',(0.01825,0.,0.002));
#7813=CARTESIAN_POINT('',(0.02125,-0.0127,0.002));
#7814=CARTESIAN_POINT('',(0.,-0.0127,0.002));
#7815=CARTESIAN_POINT('',(0.02125,-0.0175,0.002));
#7816=CARTESIAN_POINT('',(0.02125,0.,0.002));
#7817=CARTESIAN_POINT('',(0.,-0.0175,0.002));
#7818=CARTESIAN_POINT('',(0.00225,-0.0127,0.002));
#7819=CARTESIAN_POINT('',(0.00225,-0.0175,0.002));
#7820=CARTESIAN_POINT('',(0.00225,-3.90312782094782E-19,0.002));
#7821=CARTESIAN_POINT('',(0.00525,-0.0127,0.002));
#7822=CARTESIAN_POINT('',(0.,-0.0127,0.002));
#7823=CARTESIAN_POINT('',(0.00525,-0.0175,0.002));
#7824=CARTESIAN_POINT('',(0.00525,0.,0.002));
#7825=CARTESIAN_POINT('',(0.,-0.0175,0.002));
#7826=CARTESIAN_POINT('',(-0.00525,-0.0127,0.002));
#7827=CARTESIAN_POINT('',(-0.00525,-0.0175,0.002));
#7828=CARTESIAN_POINT('',(-0.00525,0.,0.002));
#7829=CARTESIAN_POINT('',(-0.00225,-0.0127,0.002));
#7830=CARTESIAN_POINT('',(-7.34366271496849E-18,-0.0127,0.002));
#7831=CARTESIAN_POINT('',(-0.00225,-0.0175,0.002));
#7832=CARTESIAN_POINT('',(-0.00225,3.90312782094781E-19,0.002));
#7833=CARTESIAN_POINT('',(0.,-0.0175,0.002));
#7834=CARTESIAN_POINT('Origin',(0.01825,-0.00375,-0.01));
#7835=CARTESIAN_POINT('',(0.01825,-0.00278889744907202,-0.01));
#7836=CARTESIAN_POINT('',(0.01825,-0.0025,-0.00882882057274445));
#7837=CARTESIAN_POINT('Origin',(0.01825,-0.01,-0.0076));
#7838=CARTESIAN_POINT('',(0.01825,-0.0025,-0.01));
#7839=CARTESIAN_POINT('',(0.01825,-0.00375,-0.01));
#7840=CARTESIAN_POINT('',(0.01825,-0.0025,-0.01));
#7841=CARTESIAN_POINT('Origin',(0.02125,-0.00375,-0.01));
#7842=CARTESIAN_POINT('',(0.02125,-0.00278889744907202,-0.01));
#7843=CARTESIAN_POINT('',(0.02125,-0.0025,-0.01));
#7844=CARTESIAN_POINT('',(0.02125,-0.00375,-0.01));
#7845=CARTESIAN_POINT('',(0.02125,-0.0025,-0.00882882057274445));
#7846=CARTESIAN_POINT('Origin',(0.02125,-0.01,-0.0076));
#7847=CARTESIAN_POINT('',(0.02125,-0.0025,-0.01));
#7848=CARTESIAN_POINT('Origin',(0.00525,-0.00375,-0.01));
#7849=CARTESIAN_POINT('',(0.00525,-0.00278889744907202,-0.01));
#7850=CARTESIAN_POINT('',(0.00525,-0.0025,-0.01));
#7851=CARTESIAN_POINT('',(0.00525,-0.00375,-0.01));
#7852=CARTESIAN_POINT('',(0.00525,-0.0025,-0.00882882057274439));
#7853=CARTESIAN_POINT('Origin',(0.00525,-0.01,-0.0076));
#7854=CARTESIAN_POINT('',(0.00525,-0.0025,-0.01));
#7855=CARTESIAN_POINT('Origin',(0.01975,-0.0175,-0.01));
#7856=CARTESIAN_POINT('',(0.01825,-0.0175,-0.01));
#7857=CARTESIAN_POINT('',(0.01825,-0.0175,-0.00882882057274447));
#7858=CARTESIAN_POINT('',(0.01825,-0.0175,-0.01));
#7859=CARTESIAN_POINT('',(0.02125,-0.0175,-0.00882882057274447));
#7860=CARTESIAN_POINT('',(-0.02675,-0.0175,-0.00882882057274447));
#7861=CARTESIAN_POINT('',(0.02125,-0.0175,-0.01));
#7862=CARTESIAN_POINT('',(0.02125,-0.0175,-0.01));
#7863=CARTESIAN_POINT('',(0.01975,-0.0175,-0.01));
#7864=CARTESIAN_POINT('Origin',(0.00375,-0.0175,-0.01));
#7865=CARTESIAN_POINT('',(0.00225,-0.0175,-0.01));
#7866=CARTESIAN_POINT('',(0.00225,-0.0175,-0.00882882057274447));
#7867=CARTESIAN_POINT('',(0.00225,-0.0175,-0.01));
#7868=CARTESIAN_POINT('',(0.00525,-0.0175,-0.00882882057274447));
#7869=CARTESIAN_POINT('',(-0.02675,-0.0175,-0.00882882057274447));
#7870=CARTESIAN_POINT('',(0.00525,-0.0175,-0.01));
#7871=CARTESIAN_POINT('',(0.00525,-0.0175,-0.01));
#7872=CARTESIAN_POINT('',(0.00375,-0.0175,-0.01));
#7873=CARTESIAN_POINT('Origin',(-0.00375,-0.0175,-0.01));
#7874=CARTESIAN_POINT('',(-0.00525,-0.0175,-0.01));
#7875=CARTESIAN_POINT('',(-0.00525,-0.0175,-0.00882882057274447));
#7876=CARTESIAN_POINT('',(-0.00525,-0.0175,-0.01));
#7877=CARTESIAN_POINT('',(-0.00225,-0.0175,-0.00882882057274447));
#7878=CARTESIAN_POINT('',(-0.02675,-0.0175,-0.00882882057274447));
#7879=CARTESIAN_POINT('',(-0.00225,-0.0175,-0.01));
#7880=CARTESIAN_POINT('',(-0.00225,-0.0175,-0.01));
#7881=CARTESIAN_POINT('',(-0.00375,-0.0175,-0.01));
#7882=CARTESIAN_POINT('Origin',(-0.02125,-0.00375,-0.01));
#7883=CARTESIAN_POINT('',(-0.02125,-0.00278889744907202,-0.01));
#7884=CARTESIAN_POINT('',(-0.02125,-0.0025,-0.00882882057274445));
#7885=CARTESIAN_POINT('Origin',(-0.02125,-0.01,-0.0076));
#7886=CARTESIAN_POINT('',(-0.02125,-0.0025,-0.01));
#7887=CARTESIAN_POINT('',(-0.02125,-0.00375,-0.01));
#7888=CARTESIAN_POINT('',(-0.02125,-0.0025,-0.01));
#7889=CARTESIAN_POINT('Origin',(-0.01825,-0.00375,-0.01));
#7890=CARTESIAN_POINT('',(-0.01825,-0.00278889744907202,-0.01));
#7891=CARTESIAN_POINT('',(-0.01825,-0.0025,-0.01));
#7892=CARTESIAN_POINT('',(-0.01825,-0.00375,-0.01));
#7893=CARTESIAN_POINT('',(-0.01825,-0.0025,-0.00882882057274445));
#7894=CARTESIAN_POINT('Origin',(-0.01825,-0.01,-0.0076));
#7895=CARTESIAN_POINT('',(-0.01825,-0.0025,-0.01));
#7896=CARTESIAN_POINT('Origin',(-0.01975,-0.0175,-0.01));
#7897=CARTESIAN_POINT('',(-0.02125,-0.0175,-0.01));
#7898=CARTESIAN_POINT('',(-0.02125,-0.0175,-0.00882882057274447));
#7899=CARTESIAN_POINT('',(-0.02125,-0.0175,-0.01));
#7900=CARTESIAN_POINT('',(-0.01825,-0.0175,-0.00882882057274447));
#7901=CARTESIAN_POINT('',(-0.02675,-0.0175,-0.00882882057274447));
#7902=CARTESIAN_POINT('',(-0.01825,-0.0175,-0.01));
#7903=CARTESIAN_POINT('',(-0.01825,-0.0175,-0.01));
#7904=CARTESIAN_POINT('',(-0.01975,-0.0175,-0.01));
#7905=CARTESIAN_POINT('Origin',(0.01975,-0.0025,-0.01));
#7906=CARTESIAN_POINT('',(-0.02675,-0.0025,-0.00882882057274445));
#7907=CARTESIAN_POINT('',(0.01975,-0.0025,-0.01));
#7908=CARTESIAN_POINT('Origin',(0.00375,-0.0025,-0.01));
#7909=CARTESIAN_POINT('',(0.00225,-0.0025,-0.00882882057274439));
#7910=CARTESIAN_POINT('',(-0.02675,-0.0025,-0.00882882057274439));
#7911=CARTESIAN_POINT('',(0.00225,-0.0025,-0.01));
#7912=CARTESIAN_POINT('',(0.00225,-0.0025,-0.01));
#7913=CARTESIAN_POINT('',(0.00375,-0.0025,-0.01));
#7914=CARTESIAN_POINT('Origin',(-0.01975,-0.0025,-0.01));
#7915=CARTESIAN_POINT('',(-0.02675,-0.0025,-0.00882882057274445));
#7916=CARTESIAN_POINT('',(-0.01975,-0.0025,-0.01));
#7917=CARTESIAN_POINT('Origin',(0.,0.,-0.01));
#7918=CARTESIAN_POINT('',(-0.02325,-0.017211102550928,-0.01));
#7919=CARTESIAN_POINT('',(-0.02325,-0.02,-0.01));
#7920=CARTESIAN_POINT('',(-0.02325,-3.46944695195361E-18,-0.01));
#7921=CARTESIAN_POINT('',(-0.02125,-0.017211102550928,-0.01));
#7922=CARTESIAN_POINT('',(-0.02675,-0.017211102550928,-0.01));
#7923=CARTESIAN_POINT('',(-0.02125,-0.01625,-0.01));
#7924=CARTESIAN_POINT('',(-0.01825,-0.017211102550928,-0.01));
#7925=CARTESIAN_POINT('',(-0.01825,-0.01625,-0.01));
#7926=CARTESIAN_POINT('',(-0.00525,-0.017211102550928,-0.01));
#7927=CARTESIAN_POINT('',(-0.02675,-0.017211102550928,-0.01));
#7928=CARTESIAN_POINT('',(-0.00525,-0.01625,-0.01));
#7929=CARTESIAN_POINT('',(-0.00225,-0.017211102550928,-0.01));
#7930=CARTESIAN_POINT('',(-0.00225,-0.01625,-0.01));
#7931=CARTESIAN_POINT('',(0.00225,-0.017211102550928,-0.01));
#7932=CARTESIAN_POINT('',(-0.02675,-0.017211102550928,-0.01));
#7933=CARTESIAN_POINT('',(0.00225,-0.01625,-0.01));
#7934=CARTESIAN_POINT('',(0.00525,-0.017211102550928,-0.01));
#7935=CARTESIAN_POINT('',(0.00525,-0.01625,-0.01));
#7936=CARTESIAN_POINT('',(0.01825,-0.017211102550928,-0.01));
#7937=CARTESIAN_POINT('',(-0.02675,-0.017211102550928,-0.01));
#7938=CARTESIAN_POINT('',(0.01825,-0.01625,-0.01));
#7939=CARTESIAN_POINT('',(0.02125,-0.017211102550928,-0.01));
#7940=CARTESIAN_POINT('',(0.02125,-0.01625,-0.01));
#7941=CARTESIAN_POINT('',(0.02325,-0.017211102550928,-0.01));
#7942=CARTESIAN_POINT('',(-0.02675,-0.017211102550928,-0.01));
#7943=CARTESIAN_POINT('',(0.02325,-0.02,-0.01));
#7944=CARTESIAN_POINT('',(0.02325,3.46944695195361E-18,-0.01));
#7945=CARTESIAN_POINT('',(0.,-0.02,-0.01));
#7946=CARTESIAN_POINT('Origin',(0.,0.,0.));
#7947=CARTESIAN_POINT('',(0.02325,0.005,0.));
#7948=CARTESIAN_POINT('',(0.02325,3.46944695195361E-18,0.));
#7949=CARTESIAN_POINT('',(-0.02325,0.005,0.));
#7950=CARTESIAN_POINT('',(-0.02325,0.005,0.));
#7951=CARTESIAN_POINT('',(-0.02325,-3.46944695195361E-18,0.));
#7952=CARTESIAN_POINT('Origin',(-0.02175,0.001,0.046));
#7953=CARTESIAN_POINT('',(-0.02175,0.005,0.032));
#7954=CARTESIAN_POINT('',(-0.02175,0.005,0.012));
#7955=CARTESIAN_POINT('',(-0.02175,0.005,0.046));
#7956=CARTESIAN_POINT('',(-0.02175,0.001,0.032));
#7957=CARTESIAN_POINT('',(-0.02175,-0.018,0.046));
#7958=CARTESIAN_POINT('',(-0.02175,0.001,0.012));
#7959=CARTESIAN_POINT('Origin',(-0.02325,-3.46944695195361E-18,0.002));
#7960=CARTESIAN_POINT('',(-0.02325,-0.00278889744907202,0.061));
#7961=CARTESIAN_POINT('Origin',(-0.02325,-0.01,0.0586));
#7962=CARTESIAN_POINT('',(-0.02325,-3.46944695195361E-18,0.061));
#7963=CARTESIAN_POINT('',(-0.02325,0.005,0.032));
#7964=CARTESIAN_POINT('',(-0.02325,0.0125,0.032));
#7965=CARTESIAN_POINT('',(-0.02325,0.005,0.012));
#7966=CARTESIAN_POINT('',(-0.02325,0.005,0.022));
#7967=CARTESIAN_POINT('',(-0.02325,0.0125,0.012));
#7968=CARTESIAN_POINT('',(-0.02325,-3.46944695195361E-18,-0.005));
#7969=CARTESIAN_POINT('Origin',(-0.02325,0.005,-0.005));
#7970=CARTESIAN_POINT('',(-0.02325,-3.46944695195361E-18,-0.01));
#7971=CARTESIAN_POINT('',(-0.02325,-3.46944695195361E-18,-0.01));
#7972=CARTESIAN_POINT('',(-0.02325,-0.00278889744907202,-0.01));
#7973=CARTESIAN_POINT('',(-0.02325,-3.46944695195361E-18,-0.01));
#7974=CARTESIAN_POINT('Origin',(-0.02325,-0.01,-0.0076));
#7975=CARTESIAN_POINT('',(-0.02325,-0.02,0.002));
#7976=CARTESIAN_POINT('Origin',(0.,-0.02,0.002));
#7977=CARTESIAN_POINT('',(0.02325,-0.02,0.002));
#7978=CARTESIAN_POINT('',(0.0155,-0.02,0.00888));
#7979=CARTESIAN_POINT('Origin',(0.0155,-0.02,0.00765));
#7980=CARTESIAN_POINT('',(-0.0155,-0.02,0.00888));
#7981=CARTESIAN_POINT('Origin',(-0.0155,-0.02,0.00765));
#7982=CARTESIAN_POINT('',(-0.0155,-0.02,0.03988));
#7983=CARTESIAN_POINT('Origin',(-0.0155,-0.02,0.03865));
#7984=CARTESIAN_POINT('',(0.0155,-0.02,0.03988));
#7985=CARTESIAN_POINT('Origin',(0.0155,-0.02,0.03865));
#7986=CARTESIAN_POINT('',(-1.53080849893419E-18,-0.02,0.03565));
#7987=CARTESIAN_POINT('Origin',(0.,-0.02,0.02315));
#7988=CARTESIAN_POINT('Origin',(0.02325,3.46944695195361E-18,0.002));
#7989=CARTESIAN_POINT('',(0.02325,-0.00278889744907202,0.061));
#7990=CARTESIAN_POINT('',(0.02325,3.46944695195361E-18,0.061));
#7991=CARTESIAN_POINT('Origin',(0.02325,-0.01,0.0586));
#7992=CARTESIAN_POINT('',(0.02325,-0.00278889744907202,-0.01));
#7993=CARTESIAN_POINT('Origin',(0.02325,-0.01,-0.0076));
#7994=CARTESIAN_POINT('',(0.02325,-3.46944695195361E-18,-0.01));
#7995=CARTESIAN_POINT('',(0.02325,3.46944695195361E-18,-0.01));
#7996=CARTESIAN_POINT('',(0.02325,-3.46944695195361E-18,-0.005));
#7997=CARTESIAN_POINT('',(0.02325,-3.46944695195361E-18,-0.01));
#7998=CARTESIAN_POINT('Origin',(0.02325,0.005,-0.005));
#7999=CARTESIAN_POINT('Origin',(6.93889390390723E-18,-0.018,0.046));
#8000=CARTESIAN_POINT('',(0.0155,-0.018,0.00888));
#8001=CARTESIAN_POINT('Origin',(0.0155,-0.018,0.00765));
#8002=CARTESIAN_POINT('',(-0.0155,-0.018,0.00888));
#8003=CARTESIAN_POINT('Origin',(-0.0155,-0.018,0.00765));
#8004=CARTESIAN_POINT('',(-0.0155,-0.018,0.03988));
#8005=CARTESIAN_POINT('Origin',(-0.0155,-0.018,0.03865));
#8006=CARTESIAN_POINT('',(0.0155,-0.018,0.03988));
#8007=CARTESIAN_POINT('Origin',(0.0155,-0.018,0.03865));
#8008=CARTESIAN_POINT('',(0.,-0.018,0.03565));
#8009=CARTESIAN_POINT('Origin',(0.,-0.018,0.02315));
#8010=CARTESIAN_POINT('Origin',(-0.01325,0.0125,0.032));
#8011=CARTESIAN_POINT('',(-0.01325,0.005,0.032));
#8012=CARTESIAN_POINT('Origin',(-0.01325,0.0125,0.012));
#8013=CARTESIAN_POINT('',(-0.01325,0.005,0.012));
#8014=CARTESIAN_POINT('Origin',(-0.01325,0.005,0.022));
#8015=CARTESIAN_POINT('Origin',(0.,-0.015,0.02315));
#8016=CARTESIAN_POINT('',(-1.53080849893419E-18,-0.015,0.03565));
#8017=CARTESIAN_POINT('Origin',(0.0155,-0.015,0.03865));
#8018=CARTESIAN_POINT('',(0.0155,-0.015,0.03988));
#8019=CARTESIAN_POINT('Origin',(-0.0155,-0.015,0.03865));
#8020=CARTESIAN_POINT('',(-0.0155,-0.015,0.03988));
#8021=CARTESIAN_POINT('Origin',(-0.0155,-0.015,0.00765));
#8022=CARTESIAN_POINT('',(-0.0155,-0.015,0.00888));
#8023=CARTESIAN_POINT('Origin',(0.0155,-0.015,0.00765));
#8024=CARTESIAN_POINT('',(0.0155,-0.015,0.00888));
#8025=CARTESIAN_POINT('Origin',(0.,-2.60208521396521E-18,-0.01));
#8026=CARTESIAN_POINT('',(0.02325,-2.60208521396521E-18,-0.005));
#8027=CARTESIAN_POINT('',(0.,-2.60208521396521E-18,-0.01));
#8028=CARTESIAN_POINT('Origin',(0.00225,-0.00375,-0.01));
#8029=CARTESIAN_POINT('',(0.00225,-0.00278889744907202,-0.01));
#8030=CARTESIAN_POINT('Origin',(0.00225,-0.01,-0.0076));
#8031=CARTESIAN_POINT('',(0.00225,-0.00375,-0.01));
#8032=CARTESIAN_POINT('Origin',(0.01825,-0.01625,-0.01));
#8033=CARTESIAN_POINT('Origin',(0.01825,-0.01,-0.0076));
#8034=CARTESIAN_POINT('Origin',(0.02125,-0.01625,-0.01));
#8035=CARTESIAN_POINT('Origin',(0.02125,-0.01,-0.0076));
#8036=CARTESIAN_POINT('Origin',(0.00225,-0.01625,-0.01));
#8037=CARTESIAN_POINT('Origin',(0.00225,-0.01,-0.0076));
#8038=CARTESIAN_POINT('Origin',(0.00525,-0.01625,-0.01));
#8039=CARTESIAN_POINT('Origin',(0.00525,-0.01,-0.0076));
#8040=CARTESIAN_POINT('Origin',(-0.00225,-0.00375,-0.01));
#8041=CARTESIAN_POINT('',(-0.00225,-0.0025,-0.00882882057274444));
#8042=CARTESIAN_POINT('',(-0.00225,-0.00278889744907202,-0.01));
#8043=CARTESIAN_POINT('Origin',(-0.00225,-0.01,-0.0076));
#8044=CARTESIAN_POINT('',(-0.00225,-0.0025,-0.01));
#8045=CARTESIAN_POINT('',(-0.00225,-0.0025,-0.01));
#8046=CARTESIAN_POINT('',(-0.00225,-0.00375,-0.01));
#8047=CARTESIAN_POINT('Origin',(-0.00375,-0.0025,-0.01));
#8048=CARTESIAN_POINT('',(-0.00525,-0.0025,-0.00882882057274445));
#8049=CARTESIAN_POINT('',(-0.02675,-0.0025,-0.00882882057274444));
#8050=CARTESIAN_POINT('',(-0.00525,-0.0025,-0.01));
#8051=CARTESIAN_POINT('',(-0.00525,-0.0025,-0.01));
#8052=CARTESIAN_POINT('',(-0.00375,-0.0025,-0.01));
#8053=CARTESIAN_POINT('Origin',(-0.00525,-0.00375,-0.01));
#8054=CARTESIAN_POINT('',(-0.00525,-0.00278889744907202,-0.01));
#8055=CARTESIAN_POINT('Origin',(-0.00525,-0.01,-0.0076));
#8056=CARTESIAN_POINT('',(-0.00525,-0.00375,-0.01));
#8057=CARTESIAN_POINT('Origin',(-0.00525,-0.01625,-0.01));
#8058=CARTESIAN_POINT('Origin',(-0.00525,-0.01,-0.0076));
#8059=CARTESIAN_POINT('Origin',(-0.00225,-0.01625,-0.01));
#8060=CARTESIAN_POINT('Origin',(-0.00225,-0.01,-0.0076));
#8061=CARTESIAN_POINT('Origin',(-0.02125,-0.01625,-0.01));
#8062=CARTESIAN_POINT('Origin',(-0.02125,-0.01,-0.0076));
#8063=CARTESIAN_POINT('Origin',(-0.01825,-0.01625,-0.01));
#8064=CARTESIAN_POINT('Origin',(-0.01825,-0.01,-0.0076));
#8065=CARTESIAN_POINT('Origin',(0.,0.,-0.01));
#8066=CARTESIAN_POINT('',(-0.02675,-0.00278889744907202,-0.01));
#8067=CARTESIAN_POINT('',(-0.02675,-0.00278889744907202,-0.01));
#8068=CARTESIAN_POINT('',(-0.02675,-0.00278889744907202,-0.01));
#8069=CARTESIAN_POINT('',(-0.02675,-0.00278889744907202,-0.01));
#8070=CARTESIAN_POINT('',(-0.02675,-0.00278889744907202,-0.01));
#8071=CARTESIAN_POINT('Origin',(-0.02675,-0.01,-0.0076));
#8072=CARTESIAN_POINT('',(0.01825,-0.0025,-0.00637117942725555));
#8073=CARTESIAN_POINT('',(0.01825,-0.00792727272727273,-0.000288105467603312));
#8074=CARTESIAN_POINT('Origin',(0.01825,-0.01,-0.0076));
#8075=CARTESIAN_POINT('',(0.02125,-0.00792727272727273,-0.000288105467603312));
#8076=CARTESIAN_POINT('',(-0.02675,-0.00792727272727273,-0.000288105467603312));
#8077=CARTESIAN_POINT('',(0.02125,-0.0025,-0.00637117942725555));
#8078=CARTESIAN_POINT('Origin',(0.02125,-0.01,-0.0076));
#8079=CARTESIAN_POINT('',(-0.02675,-0.0025,-0.00637117942725555));
#8080=CARTESIAN_POINT('',(0.00225,-0.0025,-0.0063711794272556));
#8081=CARTESIAN_POINT('',(0.00225,-0.00792727272727272,-0.000288105467603314));
#8082=CARTESIAN_POINT('Origin',(0.00225,-0.01,-0.0076));
#8083=CARTESIAN_POINT('',(0.00525,-0.00792727272727272,-0.000288105467603314));
#8084=CARTESIAN_POINT('',(-0.02675,-0.00792727272727272,-0.000288105467603312));
#8085=CARTESIAN_POINT('',(0.00525,-0.0025,-0.0063711794272556));
#8086=CARTESIAN_POINT('Origin',(0.00525,-0.01,-0.0076));
#8087=CARTESIAN_POINT('',(-0.02675,-0.0025,-0.0063711794272556));
#8088=CARTESIAN_POINT('',(0.02125,-0.0120727272727273,-0.000288105467603312));
#8089=CARTESIAN_POINT('',(0.01825,-0.0120727272727273,-0.000288105467603312));
#8090=CARTESIAN_POINT('',(-0.02675,-0.0120727272727273,-0.00028810546760331));
#8091=CARTESIAN_POINT('',(0.01825,-0.0175,-0.00637117942725553));
#8092=CARTESIAN_POINT('Origin',(0.01825,-0.01,-0.0076));
#8093=CARTESIAN_POINT('',(0.02125,-0.0175,-0.00637117942725553));
#8094=CARTESIAN_POINT('',(-0.02675,-0.0175,-0.00637117942725553));
#8095=CARTESIAN_POINT('Origin',(0.02125,-0.01,-0.0076));
#8096=CARTESIAN_POINT('',(0.00525,-0.0120727272727273,-0.000288105467603312));
#8097=CARTESIAN_POINT('',(0.00225,-0.0120727272727273,-0.000288105467603312));
#8098=CARTESIAN_POINT('',(-0.02675,-0.0120727272727273,-0.00028810546760331));
#8099=CARTESIAN_POINT('',(0.00225,-0.0175,-0.00637117942725553));
#8100=CARTESIAN_POINT('Origin',(0.00225,-0.01,-0.0076));
#8101=CARTESIAN_POINT('',(0.00525,-0.0175,-0.00637117942725553));
#8102=CARTESIAN_POINT('',(-0.02675,-0.0175,-0.00637117942725553));
#8103=CARTESIAN_POINT('Origin',(0.00525,-0.01,-0.0076));
#8104=CARTESIAN_POINT('',(-0.00525,-0.00792727272727272,-0.000288105467603314));
#8105=CARTESIAN_POINT('',(-0.00225,-0.00792727272727272,-0.000288105467603314));
#8106=CARTESIAN_POINT('',(-0.02675,-0.00792727272727272,-0.000288105467603312));
#8107=CARTESIAN_POINT('',(-0.00225,-0.0025,-0.00637117942725556));
#8108=CARTESIAN_POINT('Origin',(-0.00225,-0.01,-0.0076));
#8109=CARTESIAN_POINT('',(-0.00525,-0.0025,-0.00637117942725555));
#8110=CARTESIAN_POINT('',(-0.02675,-0.0025,-0.00637117942725556));
#8111=CARTESIAN_POINT('Origin',(-0.00525,-0.01,-0.0076));
#8112=CARTESIAN_POINT('',(-0.00225,-0.0120727272727273,-0.000288105467603309));
#8113=CARTESIAN_POINT('',(-0.00525,-0.0120727272727273,-0.000288105467603309));
#8114=CARTESIAN_POINT('',(-0.02675,-0.0120727272727273,-0.000288105467603309));
#8115=CARTESIAN_POINT('',(-0.00525,-0.0175,-0.00637117942725553));
#8116=CARTESIAN_POINT('Origin',(-0.00525,-0.01,-0.0076));
#8117=CARTESIAN_POINT('',(-0.00225,-0.0175,-0.00637117942725553));
#8118=CARTESIAN_POINT('',(-0.02675,-0.0175,-0.00637117942725553));
#8119=CARTESIAN_POINT('Origin',(-0.00225,-0.01,-0.0076));
#8120=CARTESIAN_POINT('',(-0.02125,-0.0025,-0.00637117942725555));
#8121=CARTESIAN_POINT('',(-0.02125,-0.00792727272727273,-0.000288105467603312));
#8122=CARTESIAN_POINT('Origin',(-0.02125,-0.01,-0.0076));
#8123=CARTESIAN_POINT('',(-0.01825,-0.00792727272727273,-0.000288105467603312));
#8124=CARTESIAN_POINT('',(-0.02675,-0.00792727272727273,-0.000288105467603312));
#8125=CARTESIAN_POINT('',(-0.01825,-0.0025,-0.00637117942725555));
#8126=CARTESIAN_POINT('Origin',(-0.01825,-0.01,-0.0076));
#8127=CARTESIAN_POINT('',(-0.02675,-0.0025,-0.00637117942725555));
#8128=CARTESIAN_POINT('',(-0.01825,-0.0120727272727273,-0.000288105467603312));
#8129=CARTESIAN_POINT('',(-0.02125,-0.0120727272727273,-0.000288105467603312));
#8130=CARTESIAN_POINT('',(-0.02675,-0.0120727272727273,-0.00028810546760331));
#8131=CARTESIAN_POINT('',(-0.02125,-0.0175,-0.00637117942725553));
#8132=CARTESIAN_POINT('Origin',(-0.02125,-0.01,-0.0076));
#8133=CARTESIAN_POINT('',(-0.01825,-0.0175,-0.00637117942725553));
#8134=CARTESIAN_POINT('',(-0.02675,-0.0175,-0.00637117942725553));
#8135=CARTESIAN_POINT('Origin',(-0.01825,-0.01,-0.0076));
#8136=CARTESIAN_POINT('Origin',(-0.01825,-0.01625,-0.01));
#8137=CARTESIAN_POINT('',(-0.01825,-0.0147131249905032,0.000812352359916264));
#8138=CARTESIAN_POINT('Origin',(-0.01825,-0.0127,-0.0003));
#8139=CARTESIAN_POINT('Origin',(-0.01825,-0.0127,0.00192470471983253));
#8140=CARTESIAN_POINT('',(-0.01825,-0.0175,-0.01));
#8141=CARTESIAN_POINT('Origin',(-0.01975,-0.0175,-0.01));
#8142=CARTESIAN_POINT('',(-0.02125,-0.0175,-0.01));
#8143=CARTESIAN_POINT('Origin',(-0.02125,-0.01625,-0.01));
#8144=CARTESIAN_POINT('',(-0.02125,-0.0147131249905032,0.000812352359916264));
#8145=CARTESIAN_POINT('Origin',(-0.02125,-0.0127,0.00192470471983253));
#8146=CARTESIAN_POINT('Origin',(-0.02125,-0.0127,-0.0003));
#8147=CARTESIAN_POINT('Origin',(-0.01975,-0.0025,-0.01));
#8148=CARTESIAN_POINT('',(-0.01825,-0.0025,-0.01));
#8149=CARTESIAN_POINT('',(-0.02125,-0.0025,-0.01));
#8150=CARTESIAN_POINT('Origin',(-0.01825,-0.00375,-0.01));
#8151=CARTESIAN_POINT('',(-0.01825,-0.00528687500949675,0.000812352359916264));
#8152=CARTESIAN_POINT('Origin',(-0.01825,-0.0073,0.00192470471983253));
#8153=CARTESIAN_POINT('Origin',(-0.01825,-0.0073,-0.0003));
#8154=CARTESIAN_POINT('Origin',(-0.02125,-0.00375,-0.01));
#8155=CARTESIAN_POINT('',(-0.02125,-0.00528687500949675,0.000812352359916264));
#8156=CARTESIAN_POINT('Origin',(-0.02125,-0.0073,-0.0003));
#8157=CARTESIAN_POINT('Origin',(-0.02125,-0.0073,0.00192470471983253));
#8158=CARTESIAN_POINT('Origin',(-0.00225,-0.01625,-0.01));
#8159=CARTESIAN_POINT('',(-0.00225,-0.0147131249905032,0.000812352359916279));
#8160=CARTESIAN_POINT('Origin',(-0.00225,-0.0127,-0.0003));
#8161=CARTESIAN_POINT('Origin',(-0.00225,-0.0127,0.00192470471983253));
#8162=CARTESIAN_POINT('',(-0.00225,-0.0175,-0.01));
#8163=CARTESIAN_POINT('Origin',(-0.00375,-0.0175,-0.01));
#8164=CARTESIAN_POINT('',(-0.00525,-0.0175,-0.01));
#8165=CARTESIAN_POINT('Origin',(-0.00525,-0.01625,-0.01));
#8166=CARTESIAN_POINT('',(-0.00525,-0.0147131249905032,0.000812352359916277));
#8167=CARTESIAN_POINT('Origin',(-0.00525,-0.0127,0.00192470471983253));
#8168=CARTESIAN_POINT('Origin',(-0.00525,-0.0127,-0.0003));
#8169=CARTESIAN_POINT('Origin',(-0.00525,-0.00375,-0.01));
#8170=CARTESIAN_POINT('',(-0.00525,-0.00528687500949675,0.000812352359916257));
#8171=CARTESIAN_POINT('Origin',(-0.00525,-0.0073,-0.0003));
#8172=CARTESIAN_POINT('Origin',(-0.00525,-0.0073,0.00192470471983252));
#8173=CARTESIAN_POINT('',(-0.00525,-0.0025,-0.01));
#8174=CARTESIAN_POINT('Origin',(-0.00375,-0.0025,-0.01));
#8175=CARTESIAN_POINT('',(-0.00225,-0.0025,-0.01));
#8176=CARTESIAN_POINT('Origin',(-0.00225,-0.00375,-0.01));
#8177=CARTESIAN_POINT('',(-0.00225,-0.00528687500949675,0.000812352359916256));
#8178=CARTESIAN_POINT('Origin',(-0.00225,-0.0073,0.00192470471983252));
#8179=CARTESIAN_POINT('Origin',(-0.00225,-0.0073,-0.0003));
#8180=CARTESIAN_POINT('Origin',(0.00525,-0.01625,-0.01));
#8181=CARTESIAN_POINT('',(0.00525,-0.0147131249905032,0.000812352359916264));
#8182=CARTESIAN_POINT('Origin',(0.00525,-0.0127,-0.0003));
#8183=CARTESIAN_POINT('Origin',(0.00525,-0.0127,0.00192470471983253));
#8184=CARTESIAN_POINT('',(0.00525,-0.0175,-0.01));
#8185=CARTESIAN_POINT('Origin',(0.00375,-0.0175,-0.01));
#8186=CARTESIAN_POINT('',(0.00225,-0.0175,-0.01));
#8187=CARTESIAN_POINT('Origin',(0.00225,-0.01625,-0.01));
#8188=CARTESIAN_POINT('',(0.00225,-0.0147131249905032,0.000812352359916264));
#8189=CARTESIAN_POINT('Origin',(0.00225,-0.0127,0.00192470471983253));
#8190=CARTESIAN_POINT('Origin',(0.00225,-0.0127,-0.0003));
#8191=CARTESIAN_POINT('Origin',(0.02125,-0.01625,-0.01));
#8192=CARTESIAN_POINT('',(0.02125,-0.0147131249905032,0.000812352359916264));
#8193=CARTESIAN_POINT('Origin',(0.02125,-0.0127,-0.0003));
#8194=CARTESIAN_POINT('Origin',(0.02125,-0.0127,0.00192470471983253));
#8195=CARTESIAN_POINT('',(0.02125,-0.0175,-0.01));
#8196=CARTESIAN_POINT('Origin',(0.01975,-0.0175,-0.01));
#8197=CARTESIAN_POINT('',(0.01825,-0.0175,-0.01));
#8198=CARTESIAN_POINT('Origin',(0.01825,-0.01625,-0.01));
#8199=CARTESIAN_POINT('',(0.01825,-0.0147131249905032,0.000812352359916264));
#8200=CARTESIAN_POINT('Origin',(0.01825,-0.0127,0.00192470471983253));
#8201=CARTESIAN_POINT('Origin',(0.01825,-0.0127,-0.0003));
#8202=CARTESIAN_POINT('Origin',(0.00375,-0.0025,-0.01));
#8203=CARTESIAN_POINT('',(0.00525,-0.0025,-0.01));
#8204=CARTESIAN_POINT('',(0.00225,-0.0025,-0.01));
#8205=CARTESIAN_POINT('Origin',(0.00525,-0.00375,-0.01));
#8206=CARTESIAN_POINT('',(0.00525,-0.00528687500949675,0.000812352359916255));
#8207=CARTESIAN_POINT('Origin',(0.00525,-0.0073,0.00192470471983252));
#8208=CARTESIAN_POINT('Origin',(0.00525,-0.0073,-0.0003));
#8209=CARTESIAN_POINT('Origin',(0.00225,-0.00375,-0.01));
#8210=CARTESIAN_POINT('',(0.00225,-0.00528687500949675,0.000812352359916255));
#8211=CARTESIAN_POINT('Origin',(0.00225,-0.0073,-0.0003));
#8212=CARTESIAN_POINT('Origin',(0.00225,-0.0073,0.00192470471983252));
#8213=CARTESIAN_POINT('Origin',(0.01975,-0.0025,-0.01));
#8214=CARTESIAN_POINT('',(0.02125,-0.0025,-0.01));
#8215=CARTESIAN_POINT('',(0.01825,-0.0025,-0.01));
#8216=CARTESIAN_POINT('Origin',(0.02125,-0.00375,-0.01));
#8217=CARTESIAN_POINT('',(0.02125,-0.00528687500949675,0.000812352359916264));
#8218=CARTESIAN_POINT('Origin',(0.02125,-0.0073,0.00192470471983253));
#8219=CARTESIAN_POINT('Origin',(0.02125,-0.0073,-0.0003));
#8220=CARTESIAN_POINT('Origin',(0.01825,-0.00375,-0.01));
#8221=CARTESIAN_POINT('',(0.01825,-0.00528687500949675,0.000812352359916264));
#8222=CARTESIAN_POINT('Origin',(0.01825,-0.0073,-0.0003));
#8223=CARTESIAN_POINT('Origin',(0.01825,-0.0073,0.00192470471983253));
#8224=CARTESIAN_POINT('Origin',(-0.02675,-0.0127,0.00192470471983253));
#8225=CARTESIAN_POINT('',(-0.00375,-0.0147131249905032,0.000812352359916278));
#8226=CARTESIAN_POINT('Origin',(-0.00375,-0.0127,-0.0003));
#8227=CARTESIAN_POINT('Origin',(-0.02675,-0.0127,0.00192470471983253));
#8228=CARTESIAN_POINT('',(0.00375,-0.0147131249905032,0.000812352359916264));
#8229=CARTESIAN_POINT('Origin',(0.00375,-0.0127,-0.0003));
#8230=CARTESIAN_POINT('Origin',(-0.02675,-0.0127,0.00192470471983253));
#8231=CARTESIAN_POINT('',(0.01975,-0.0147131249905032,0.000812352359916264));
#8232=CARTESIAN_POINT('Origin',(0.01975,-0.0127,-0.0003));
#8233=CARTESIAN_POINT('Origin',(-0.02675,-0.0073,0.00192470471983253));
#8234=CARTESIAN_POINT('',(0.01975,-0.00528687500949675,0.000812352359916264));
#8235=CARTESIAN_POINT('Origin',(0.,-0.0073,-0.0003));
#8236=CARTESIAN_POINT('Origin',(-0.02675,-0.0073,0.00192470471983252));
#8237=CARTESIAN_POINT('',(0.00375,-0.00528687500949675,0.000812352359916255));
#8238=CARTESIAN_POINT('Origin',(-2.11058022910511E-18,-0.0073,-0.0003));
#8239=CARTESIAN_POINT('Origin',(-0.02675,-0.0073,0.00192470471983252));
#8240=CARTESIAN_POINT('',(-0.00375,-0.00528687500949675,0.000812352359916257));
#8241=CARTESIAN_POINT('Origin',(-0.00375,-0.0073,-0.0003));
#8242=CARTESIAN_POINT('Origin',(-0.02675,-0.0073,0.00192470471983253));
#8243=CARTESIAN_POINT('',(-0.01975,-0.00528687500949675,0.000812352359916264));
#8244=CARTESIAN_POINT('Origin',(0.,-0.0073,-0.0003));
#8245=CARTESIAN_POINT('Origin',(-0.02675,-0.0127,0.00192470471983253));
#8246=CARTESIAN_POINT('',(-0.01975,-0.0147131249905032,0.000812352359916264));
#8247=CARTESIAN_POINT('Origin',(-0.01975,-0.0127,-0.0003));
#8248=CARTESIAN_POINT('Origin',(0.01825,-0.00375,0.061));
#8249=CARTESIAN_POINT('',(0.01825,-0.0025,0.0598288205727444));
#8250=CARTESIAN_POINT('',(0.01825,-0.00278889744907202,0.061));
#8251=CARTESIAN_POINT('Origin',(0.01825,-0.01,0.0586));
#8252=CARTESIAN_POINT('',(0.01825,-0.0025,0.061));
#8253=CARTESIAN_POINT('',(0.01825,-0.0025,0.061));
#8254=CARTESIAN_POINT('',(0.01825,-0.00375,0.061));
#8255=CARTESIAN_POINT('Origin',(0.01975,-0.0025,0.061));
#8256=CARTESIAN_POINT('',(0.02125,-0.0025,0.0598288205727444));
#8257=CARTESIAN_POINT('',(0.02675,-0.0025,0.0598288205727444));
#8258=CARTESIAN_POINT('',(0.02125,-0.0025,0.061));
#8259=CARTESIAN_POINT('',(0.02125,-0.0025,0.061));
#8260=CARTESIAN_POINT('',(0.01975,-0.0025,0.061));
#8261=CARTESIAN_POINT('Origin',(0.02125,-0.00375,0.061));
#8262=CARTESIAN_POINT('',(0.02125,-0.00278889744907202,0.061));
#8263=CARTESIAN_POINT('Origin',(0.02125,-0.01,0.0586));
#8264=CARTESIAN_POINT('',(0.02125,-0.00375,0.061));
#8265=CARTESIAN_POINT('Origin',(0.00375,-0.0025,0.061));
#8266=CARTESIAN_POINT('',(0.00525,-0.0025,0.0598288205727444));
#8267=CARTESIAN_POINT('',(0.02675,-0.0025,0.0598288205727444));
#8268=CARTESIAN_POINT('',(0.00525,-0.0025,0.061));
#8269=CARTESIAN_POINT('',(0.00525,-0.0025,0.061));
#8270=CARTESIAN_POINT('',(0.00375,-0.0025,0.061));
#8271=CARTESIAN_POINT('Origin',(0.00525,-0.00375,0.061));
#8272=CARTESIAN_POINT('',(0.00525,-0.00278889744907202,0.061));
#8273=CARTESIAN_POINT('Origin',(0.00525,-0.01,0.0586));
#8274=CARTESIAN_POINT('',(0.00525,-0.00375,0.061));
#8275=CARTESIAN_POINT('Origin',(-0.00525,-0.01625,0.061));
#8276=CARTESIAN_POINT('Origin',(-0.00525,-0.01,0.0586));
#8277=CARTESIAN_POINT('Origin',(-0.00525,-0.00375,0.061));
#8278=CARTESIAN_POINT('',(-0.00525,-0.0025,0.0598288205727444));
#8279=CARTESIAN_POINT('',(-0.00525,-0.00278889744907202,0.061));
#8280=CARTESIAN_POINT('Origin',(-0.00525,-0.01,0.0586));
#8281=CARTESIAN_POINT('',(-0.00525,-0.0025,0.061));
#8282=CARTESIAN_POINT('',(-0.00525,-0.0025,0.061));
#8283=CARTESIAN_POINT('',(-0.00525,-0.00375,0.061));
#8284=CARTESIAN_POINT('Origin',(-0.00375,-0.0025,0.061));
#8285=CARTESIAN_POINT('',(0.02675,-0.0025,0.0598288205727444));
#8286=CARTESIAN_POINT('',(-0.00375,-0.0025,0.061));
#8287=CARTESIAN_POINT('Origin',(-0.02125,-0.00375,0.061));
#8288=CARTESIAN_POINT('',(-0.02125,-0.0025,0.0598288205727444));
#8289=CARTESIAN_POINT('',(-0.02125,-0.00278889744907202,0.061));
#8290=CARTESIAN_POINT('Origin',(-0.02125,-0.01,0.0586));
#8291=CARTESIAN_POINT('',(-0.02125,-0.0025,0.061));
#8292=CARTESIAN_POINT('',(-0.02125,-0.0025,0.061));
#8293=CARTESIAN_POINT('',(-0.02125,-0.00375,0.061));
#8294=CARTESIAN_POINT('Origin',(-0.01975,-0.0025,0.061));
#8295=CARTESIAN_POINT('',(-0.01825,-0.0025,0.0598288205727444));
#8296=CARTESIAN_POINT('',(0.02675,-0.0025,0.0598288205727444));
#8297=CARTESIAN_POINT('',(-0.01825,-0.0025,0.061));
#8298=CARTESIAN_POINT('',(-0.01825,-0.0025,0.061));
#8299=CARTESIAN_POINT('',(-0.01975,-0.0025,0.061));
#8300=CARTESIAN_POINT('Origin',(-0.01825,-0.00375,0.061));
#8301=CARTESIAN_POINT('',(-0.01825,-0.00278889744907202,0.061));
#8302=CARTESIAN_POINT('Origin',(-0.01825,-0.01,0.0586));
#8303=CARTESIAN_POINT('',(-0.01825,-0.00375,0.061));
#8304=CARTESIAN_POINT('Origin',(0.00375,-0.0175,0.061));
#8305=CARTESIAN_POINT('',(0.02675,-0.0175,0.0598288205727445));
#8306=CARTESIAN_POINT('Origin',(-0.01975,-0.0175,0.061));
#8307=CARTESIAN_POINT('',(0.02675,-0.0175,0.0598288205727445));
#8308=CARTESIAN_POINT('Origin',(0.01975,-0.0175,0.061));
#8309=CARTESIAN_POINT('',(0.02675,-0.0175,0.0598288205727445));
#8310=CARTESIAN_POINT('Origin',(-3.46944695195361E-18,0.,0.061));
#8311=CARTESIAN_POINT('',(0.02675,-0.00278889744907202,0.061));
#8312=CARTESIAN_POINT('',(0.02675,-0.00278889744907202,0.061));
#8313=CARTESIAN_POINT('',(0.02675,-0.00278889744907202,0.061));
#8314=CARTESIAN_POINT('',(0.02675,-0.00278889744907202,0.061));
#8315=CARTESIAN_POINT('',(0.02675,-0.00278889744907202,0.061));
#8316=CARTESIAN_POINT('Origin',(0.02675,-0.01,0.0586));
#8317=CARTESIAN_POINT('',(0.00225,-0.0175,0.0573711794272556));
#8318=CARTESIAN_POINT('',(0.00225,-0.0120727272727273,0.0512881054676033));
#8319=CARTESIAN_POINT('Origin',(0.00225,-0.01,0.0586));
#8320=CARTESIAN_POINT('',(0.00525,-0.0120727272727273,0.0512881054676033));
#8321=CARTESIAN_POINT('',(0.02675,-0.0120727272727273,0.0512881054676033));
#8322=CARTESIAN_POINT('',(0.00525,-0.0175,0.0573711794272556));
#8323=CARTESIAN_POINT('Origin',(0.00525,-0.01,0.0586));
#8324=CARTESIAN_POINT('',(0.02675,-0.0175,0.0573711794272556));
#8325=CARTESIAN_POINT('',(0.02125,-0.00792727272727272,0.0512881054676033));
#8326=CARTESIAN_POINT('',(0.01825,-0.00792727272727272,0.0512881054676033));
#8327=CARTESIAN_POINT('',(0.02675,-0.00792727272727272,0.0512881054676033));
#8328=CARTESIAN_POINT('',(0.01825,-0.0025,0.0573711794272556));
#8329=CARTESIAN_POINT('Origin',(0.01825,-0.01,0.0586));
#8330=CARTESIAN_POINT('',(0.02125,-0.0025,0.0573711794272556));
#8331=CARTESIAN_POINT('',(0.02675,-0.0025,0.0573711794272556));
#8332=CARTESIAN_POINT('Origin',(0.02125,-0.01,0.0586));
#8333=CARTESIAN_POINT('',(0.00525,-0.00792727272727272,0.0512881054676033));
#8334=CARTESIAN_POINT('',(0.00225,-0.00792727272727272,0.0512881054676033));
#8335=CARTESIAN_POINT('',(0.02675,-0.00792727272727272,0.0512881054676033));
#8336=CARTESIAN_POINT('',(0.00225,-0.0025,0.0573711794272556));
#8337=CARTESIAN_POINT('Origin',(0.00225,-0.01,0.0586));
#8338=CARTESIAN_POINT('',(0.00525,-0.0025,0.0573711794272556));
#8339=CARTESIAN_POINT('',(0.02675,-0.0025,0.0573711794272556));
#8340=CARTESIAN_POINT('Origin',(0.00525,-0.01,0.0586));
#8341=CARTESIAN_POINT('',(-0.00525,-0.0120727272727273,0.0512881054676033));
#8342=CARTESIAN_POINT('',(-0.00225,-0.0120727272727273,0.0512881054676033));
#8343=CARTESIAN_POINT('',(0.02675,-0.0120727272727273,0.0512881054676033));
#8344=CARTESIAN_POINT('',(-0.00225,-0.0175,0.0573711794272556));
#8345=CARTESIAN_POINT('Origin',(-0.00225,-0.01,0.0586));
#8346=CARTESIAN_POINT('',(-0.00525,-0.0175,0.0573711794272556));
#8347=CARTESIAN_POINT('',(0.02675,-0.0175,0.0573711794272556));
#8348=CARTESIAN_POINT('Origin',(-0.00525,-0.01,0.0586));
#8349=CARTESIAN_POINT('',(-0.00225,-0.00792727272727272,0.0512881054676033));
#8350=CARTESIAN_POINT('',(-0.00525,-0.00792727272727272,0.0512881054676033));
#8351=CARTESIAN_POINT('',(0.02675,-0.00792727272727272,0.0512881054676033));
#8352=CARTESIAN_POINT('',(-0.00525,-0.0025,0.0573711794272556));
#8353=CARTESIAN_POINT('Origin',(-0.00525,-0.01,0.0586));
#8354=CARTESIAN_POINT('',(-0.00225,-0.0025,0.0573711794272556));
#8355=CARTESIAN_POINT('',(0.02675,-0.0025,0.0573711794272556));
#8356=CARTESIAN_POINT('Origin',(-0.00225,-0.01,0.0586));
#8357=CARTESIAN_POINT('',(-0.02125,-0.0175,0.0573711794272556));
#8358=CARTESIAN_POINT('',(-0.02125,-0.0120727272727273,0.0512881054676033));
#8359=CARTESIAN_POINT('Origin',(-0.02125,-0.01,0.0586));
#8360=CARTESIAN_POINT('',(-0.01825,-0.0120727272727273,0.0512881054676033));
#8361=CARTESIAN_POINT('',(0.02675,-0.0120727272727273,0.0512881054676033));
#8362=CARTESIAN_POINT('',(-0.01825,-0.0175,0.0573711794272556));
#8363=CARTESIAN_POINT('Origin',(-0.01825,-0.01,0.0586));
#8364=CARTESIAN_POINT('',(0.02675,-0.0175,0.0573711794272556));
#8365=CARTESIAN_POINT('',(-0.01825,-0.00792727272727272,0.0512881054676033));
#8366=CARTESIAN_POINT('',(-0.02125,-0.00792727272727272,0.0512881054676033));
#8367=CARTESIAN_POINT('',(0.02675,-0.00792727272727272,0.0512881054676033));
#8368=CARTESIAN_POINT('',(-0.02125,-0.0025,0.0573711794272556));
#8369=CARTESIAN_POINT('Origin',(-0.02125,-0.01,0.0586));
#8370=CARTESIAN_POINT('',(-0.01825,-0.0025,0.0573711794272556));
#8371=CARTESIAN_POINT('',(0.02675,-0.0025,0.0573711794272556));
#8372=CARTESIAN_POINT('Origin',(-0.01825,-0.01,0.0586));
#8373=CARTESIAN_POINT('',(0.01825,-0.0175,0.0573711794272556));
#8374=CARTESIAN_POINT('',(0.01825,-0.0120727272727273,0.0512881054676033));
#8375=CARTESIAN_POINT('Origin',(0.01825,-0.01,0.0586));
#8376=CARTESIAN_POINT('',(0.02125,-0.0120727272727273,0.0512881054676033));
#8377=CARTESIAN_POINT('',(0.02675,-0.0120727272727273,0.0512881054676033));
#8378=CARTESIAN_POINT('',(0.02125,-0.0175,0.0573711794272556));
#8379=CARTESIAN_POINT('Origin',(0.02125,-0.01,0.0586));
#8380=CARTESIAN_POINT('',(0.02675,-0.0175,0.0573711794272556));
#8381=CARTESIAN_POINT('Origin',(0.01975,-0.0175,0.061));
#8382=CARTESIAN_POINT('',(0.02125,-0.0175,0.061));
#8383=CARTESIAN_POINT('',(0.01825,-0.0175,0.061));
#8384=CARTESIAN_POINT('Origin',(0.02125,-0.01625,0.061));
#8385=CARTESIAN_POINT('',(0.02125,-0.015,0.0490752952801675));
#8386=CARTESIAN_POINT('Origin',(0.02125,-0.0127,0.0490752952801675));
#8387=CARTESIAN_POINT('',(0.02125,-0.015,0.0483));
#8388=CARTESIAN_POINT('',(0.02125,-0.015,0.061));
#8389=CARTESIAN_POINT('Origin',(0.02125,-0.0127,0.0483));
#8390=CARTESIAN_POINT('Origin',(0.01975,-0.015,0.061));
#8391=CARTESIAN_POINT('',(0.01825,-0.015,0.0490752952801675));
#8392=CARTESIAN_POINT('',(0.01825,-0.015,0.0483));
#8393=CARTESIAN_POINT('',(0.01825,-0.015,0.061));
#8394=CARTESIAN_POINT('',(0.01975,-0.015,0.0483));
#8395=CARTESIAN_POINT('',(0.01975,-0.015,0.0490752952801675));
#8396=CARTESIAN_POINT('Origin',(0.01825,-0.01625,0.061));
#8397=CARTESIAN_POINT('Origin',(0.01825,-0.0127,0.0483));
#8398=CARTESIAN_POINT('Origin',(0.01825,-0.0127,0.0490752952801675));
#8399=CARTESIAN_POINT('Origin',(-0.01975,-0.005,0.061));
#8400=CARTESIAN_POINT('',(-0.01825,-0.005,0.0490752952801675));
#8401=CARTESIAN_POINT('',(-0.01825,-0.005,0.0483));
#8402=CARTESIAN_POINT('',(-0.01825,-0.005,0.061));
#8403=CARTESIAN_POINT('',(-0.02125,-0.005,0.0483));
#8404=CARTESIAN_POINT('',(-0.02125,-0.005,0.0483));
#8405=CARTESIAN_POINT('',(-0.02125,-0.005,0.0490752952801675));
#8406=CARTESIAN_POINT('',(-0.02125,-0.005,0.061));
#8407=CARTESIAN_POINT('',(-0.01825,-0.005,0.0490752952801675));
#8408=CARTESIAN_POINT('Origin',(-0.01825,-0.00375,0.061));
#8409=CARTESIAN_POINT('Origin',(-0.01825,-0.0073,0.0490752952801675));
#8410=CARTESIAN_POINT('',(-0.01825,-0.0025,0.061));
#8411=CARTESIAN_POINT('Origin',(-0.01825,-0.0073,0.0483));
#8412=CARTESIAN_POINT('Origin',(-0.01975,-0.0025,0.061));
#8413=CARTESIAN_POINT('',(-0.02125,-0.0025,0.061));
#8414=CARTESIAN_POINT('Origin',(-0.02125,-0.00375,0.061));
#8415=CARTESIAN_POINT('Origin',(-0.02125,-0.0073,0.0490752952801675));
#8416=CARTESIAN_POINT('Origin',(-0.02125,-0.0073,0.0483));
#8417=CARTESIAN_POINT('Origin',(-0.01975,-0.0175,0.061));
#8418=CARTESIAN_POINT('',(-0.01825,-0.0175,0.061));
#8419=CARTESIAN_POINT('',(-0.02125,-0.0175,0.061));
#8420=CARTESIAN_POINT('Origin',(-0.01825,-0.01625,0.061));
#8421=CARTESIAN_POINT('',(-0.01825,-0.015,0.0490752952801675));
#8422=CARTESIAN_POINT('Origin',(-0.01825,-0.0127,0.0490752952801675));
#8423=CARTESIAN_POINT('',(-0.01825,-0.015,0.0483));
#8424=CARTESIAN_POINT('',(-0.01825,-0.015,0.061));
#8425=CARTESIAN_POINT('Origin',(-0.01825,-0.0127,0.0483));
#8426=CARTESIAN_POINT('Origin',(-0.01975,-0.015,0.061));
#8427=CARTESIAN_POINT('',(-0.02125,-0.015,0.0490752952801675));
#8428=CARTESIAN_POINT('',(-0.02125,-0.015,0.0483));
#8429=CARTESIAN_POINT('',(-0.02125,-0.015,0.061));
#8430=CARTESIAN_POINT('',(-0.01975,-0.015,0.0483));
#8431=CARTESIAN_POINT('',(-0.01975,-0.015,0.0490752952801675));
#8432=CARTESIAN_POINT('Origin',(-0.02125,-0.01625,0.061));
#8433=CARTESIAN_POINT('Origin',(-0.02125,-0.0127,0.0483));
#8434=CARTESIAN_POINT('Origin',(-0.02125,-0.0127,0.0490752952801675));
#8435=CARTESIAN_POINT('Origin',(-0.00375,-0.005,0.061));
#8436=CARTESIAN_POINT('',(-0.00225,-0.005,0.0490752952801675));
#8437=CARTESIAN_POINT('',(-0.00225,-0.005,0.0483));
#8438=CARTESIAN_POINT('',(-0.00225,-0.005,0.061));
#8439=CARTESIAN_POINT('',(-0.00525,-0.005,0.0483));
#8440=CARTESIAN_POINT('',(-0.00525,-0.005,0.0483));
#8441=CARTESIAN_POINT('',(-0.00525,-0.005,0.0490752952801675));
#8442=CARTESIAN_POINT('',(-0.00525,-0.005,0.061));
#8443=CARTESIAN_POINT('',(-0.00225,-0.005,0.0490752952801675));
#8444=CARTESIAN_POINT('Origin',(-0.00225,-0.00375,0.061));
#8445=CARTESIAN_POINT('Origin',(-0.00225,-0.0073,0.0490752952801675));
#8446=CARTESIAN_POINT('',(-0.00225,-0.0025,0.061));
#8447=CARTESIAN_POINT('Origin',(-0.00225,-0.0073,0.0483));
#8448=CARTESIAN_POINT('Origin',(-0.00375,-0.0025,0.061));
#8449=CARTESIAN_POINT('',(-0.00525,-0.0025,0.061));
#8450=CARTESIAN_POINT('Origin',(-0.00525,-0.00375,0.061));
#8451=CARTESIAN_POINT('Origin',(-0.00525,-0.0073,0.0490752952801675));
#8452=CARTESIAN_POINT('Origin',(-0.00525,-0.0073,0.0483));
#8453=CARTESIAN_POINT('Origin',(-0.00375,-0.015,0.061));
#8454=CARTESIAN_POINT('',(-0.00525,-0.015,0.0490752952801675));
#8455=CARTESIAN_POINT('',(-0.00525,-0.015,0.0483));
#8456=CARTESIAN_POINT('',(-0.00525,-0.015,0.061));
#8457=CARTESIAN_POINT('',(-0.00225,-0.015,0.0483));
#8458=CARTESIAN_POINT('',(-0.00225,-0.015,0.0483));
#8459=CARTESIAN_POINT('',(-0.00225,-0.015,0.0490752952801675));
#8460=CARTESIAN_POINT('',(-0.00225,-0.015,0.061));
#8461=CARTESIAN_POINT('',(-0.00525,-0.015,0.0490752952801675));
#8462=CARTESIAN_POINT('Origin',(-0.00525,-0.01625,0.061));
#8463=CARTESIAN_POINT('Origin',(-0.00525,-0.0127,0.0490752952801675));
#8464=CARTESIAN_POINT('',(-0.00525,-0.0175,0.061));
#8465=CARTESIAN_POINT('Origin',(-0.00525,-0.0127,0.0483));
#8466=CARTESIAN_POINT('Origin',(-0.00375,-0.0175,0.061));
#8467=CARTESIAN_POINT('',(-0.00225,-0.0175,0.061));
#8468=CARTESIAN_POINT('Origin',(-0.00225,-0.01625,0.061));
#8469=CARTESIAN_POINT('Origin',(-0.00225,-0.0127,0.0490752952801675));
#8470=CARTESIAN_POINT('Origin',(-0.00225,-0.0127,0.0483));
#8471=CARTESIAN_POINT('Origin',(0.00375,-0.005,0.061));
#8472=CARTESIAN_POINT('',(0.00525,-0.005,0.0490752952801675));
#8473=CARTESIAN_POINT('',(0.00525,-0.005,0.0483));
#8474=CARTESIAN_POINT('',(0.00525,-0.005,0.061));
#8475=CARTESIAN_POINT('',(0.00225,-0.005,0.0483));
#8476=CARTESIAN_POINT('',(0.00225,-0.005,0.0483));
#8477=CARTESIAN_POINT('',(0.00225,-0.005,0.0490752952801675));
#8478=CARTESIAN_POINT('',(0.00225,-0.005,0.061));
#8479=CARTESIAN_POINT('',(0.00525,-0.005,0.0490752952801675));
#8480=CARTESIAN_POINT('Origin',(0.00525,-0.00375,0.061));
#8481=CARTESIAN_POINT('Origin',(0.00525,-0.0073,0.0490752952801675));
#8482=CARTESIAN_POINT('',(0.00525,-0.0025,0.061));
#8483=CARTESIAN_POINT('Origin',(0.00525,-0.0073,0.0483));
#8484=CARTESIAN_POINT('Origin',(0.00375,-0.0025,0.061));
#8485=CARTESIAN_POINT('',(0.00225,-0.0025,0.061));
#8486=CARTESIAN_POINT('Origin',(0.00225,-0.00375,0.061));
#8487=CARTESIAN_POINT('Origin',(0.00225,-0.0073,0.0490752952801675));
#8488=CARTESIAN_POINT('Origin',(0.00225,-0.0073,0.0483));
#8489=CARTESIAN_POINT('Origin',(0.01975,-0.005,0.061));
#8490=CARTESIAN_POINT('',(0.02125,-0.005,0.0490752952801675));
#8491=CARTESIAN_POINT('',(0.02125,-0.005,0.0483));
#8492=CARTESIAN_POINT('',(0.02125,-0.005,0.061));
#8493=CARTESIAN_POINT('',(0.01825,-0.005,0.0483));
#8494=CARTESIAN_POINT('',(0.01825,-0.005,0.0483));
#8495=CARTESIAN_POINT('',(0.01825,-0.005,0.0490752952801675));
#8496=CARTESIAN_POINT('',(0.01825,-0.005,0.061));
#8497=CARTESIAN_POINT('',(0.02125,-0.005,0.0490752952801675));
#8498=CARTESIAN_POINT('Origin',(0.02125,-0.00375,0.061));
#8499=CARTESIAN_POINT('Origin',(0.02125,-0.0073,0.0490752952801675));
#8500=CARTESIAN_POINT('',(0.02125,-0.0025,0.061));
#8501=CARTESIAN_POINT('Origin',(0.02125,-0.0073,0.0483));
#8502=CARTESIAN_POINT('Origin',(0.01975,-0.0025,0.061));
#8503=CARTESIAN_POINT('',(0.01825,-0.0025,0.061));
#8504=CARTESIAN_POINT('Origin',(0.01825,-0.00375,0.061));
#8505=CARTESIAN_POINT('Origin',(0.01825,-0.0073,0.0490752952801675));
#8506=CARTESIAN_POINT('Origin',(0.01825,-0.0073,0.0483));
#8507=CARTESIAN_POINT('Origin',(0.00375,-0.0175,0.061));
#8508=CARTESIAN_POINT('',(0.00525,-0.0175,0.061));
#8509=CARTESIAN_POINT('',(0.00225,-0.0175,0.061));
#8510=CARTESIAN_POINT('Origin',(0.00525,-0.01625,0.061));
#8511=CARTESIAN_POINT('',(0.00525,-0.015,0.0490752952801675));
#8512=CARTESIAN_POINT('Origin',(0.00525,-0.0127,0.0490752952801675));
#8513=CARTESIAN_POINT('',(0.00525,-0.015,0.0483));
#8514=CARTESIAN_POINT('',(0.00525,-0.015,0.061));
#8515=CARTESIAN_POINT('Origin',(0.00525,-0.0127,0.0483));
#8516=CARTESIAN_POINT('Origin',(0.00375,-0.015,0.061));
#8517=CARTESIAN_POINT('',(0.00225,-0.015,0.0490752952801675));
#8518=CARTESIAN_POINT('',(0.00225,-0.015,0.0483));
#8519=CARTESIAN_POINT('',(0.00225,-0.015,0.061));
#8520=CARTESIAN_POINT('',(0.00375,-0.015,0.0483));
#8521=CARTESIAN_POINT('',(0.00375,-0.015,0.0490752952801675));
#8522=CARTESIAN_POINT('Origin',(0.00225,-0.01625,0.061));
#8523=CARTESIAN_POINT('Origin',(0.00225,-0.0127,0.0483));
#8524=CARTESIAN_POINT('Origin',(0.00225,-0.0127,0.0490752952801675));
#8525=CARTESIAN_POINT('Origin',(-0.01975,-0.0127,0.0483));
#8526=CARTESIAN_POINT('Origin',(0.,-0.0127,0.0483));
#8527=CARTESIAN_POINT('Origin',(0.00375,-0.0127,0.0483));
#8528=CARTESIAN_POINT('Origin',(0.01975,-0.0127,0.0483));
#8529=CARTESIAN_POINT('Origin',(0.,-0.0073,0.0483));
#8530=CARTESIAN_POINT('Origin',(0.,-0.0073,0.0483));
#8531=CARTESIAN_POINT('Origin',(0.,-0.0073,0.0483));
#8532=CARTESIAN_POINT('Origin',(0.,-0.0073,0.0483));
#8533=CARTESIAN_POINT('Origin',(0.02675,-0.0127,0.0490752952801675));
#8534=CARTESIAN_POINT('Origin',(0.02675,-0.0073,0.0490752952801675));
#8535=CARTESIAN_POINT('Origin',(0.02675,-0.0073,0.0490752952801675));
#8536=CARTESIAN_POINT('Origin',(0.02675,-0.0127,0.0490752952801675));
#8537=CARTESIAN_POINT('Origin',(0.02675,-0.0073,0.0490752952801675));
#8538=CARTESIAN_POINT('Origin',(0.02675,-0.0127,0.0490752952801675));
#8539=CARTESIAN_POINT('Origin',(0.02675,-0.0073,0.0490752952801675));
#8540=CARTESIAN_POINT('Origin',(0.02675,-0.0127,0.0490752952801675));
#8541=CARTESIAN_POINT('Origin',(0.,0.005,-0.005));
#8542=CARTESIAN_POINT('',(0.,0.,0.));
#8543=CARTESIAN_POINT('Origin',(0.0735500000002153,-0.0149750000000067,
0.02565));
#8544=CARTESIAN_POINT('',(0.0735500000002123,-0.0172000000000067,-0.00982499999999996));
#8545=CARTESIAN_POINT('',(0.073550000000219,-0.0122000000000067,-0.014825));
#8546=CARTESIAN_POINT('Origin',(0.073550000000219,-0.0122000000000066,-0.00982499999999993));
#8547=CARTESIAN_POINT('',(0.073550000000225,-0.00775000000000667,-0.014825));
#8548=CARTESIAN_POINT('',(0.073550000000219,-0.0122000000000067,-0.014825));
#8549=CARTESIAN_POINT('',(0.0735500000002317,-0.00275000000000667,-0.00982499999999996));
#8550=CARTESIAN_POINT('Origin',(0.073550000000225,-0.0077500000000067,-0.00982499999999995));
#8551=CARTESIAN_POINT('',(0.0735500000002317,-0.00275000000000663,0.061125));
#8552=CARTESIAN_POINT('',(0.0735500000002317,-0.00275000000000667,-0.00982499999999996));
#8553=CARTESIAN_POINT('',(0.073550000000225,-0.00775000000000667,0.066125));
#8554=CARTESIAN_POINT('Origin',(0.0735500000002251,-0.00775000000000667,
0.061125));
#8555=CARTESIAN_POINT('',(0.073550000000219,-0.0122000000000067,0.066125));
#8556=CARTESIAN_POINT('',(0.073550000000225,-0.00775000000000667,0.066125));
#8557=CARTESIAN_POINT('',(0.0735500000002123,-0.0172000000000066,0.061125));
#8558=CARTESIAN_POINT('Origin',(0.073550000000219,-0.0122000000000066,0.061125));
#8559=CARTESIAN_POINT('',(0.0735500000002123,-0.0172000000000067,0.053125));
#8560=CARTESIAN_POINT('',(0.0735500000002123,-0.0172000000000066,0.061125));
#8561=CARTESIAN_POINT('',(0.0735500000002056,-0.0222000000000067,0.048125));
#8562=CARTESIAN_POINT('Origin',(0.0735500000002056,-0.0222000000000067,
0.053125));
#8563=CARTESIAN_POINT('',(0.0735500000001988,-0.0272000000000067,0.0431250000000001));
#8564=CARTESIAN_POINT('Origin',(0.0735500000002055,-0.0222000000000067,
0.043125));
#8565=CARTESIAN_POINT('',(0.0735500000001988,-0.0272000000000067,0.00817500000000003));
#8566=CARTESIAN_POINT('',(0.0735500000001988,-0.0272000000000067,0.0431250000000001));
#8567=CARTESIAN_POINT('',(0.0735500000002056,-0.0222000000000067,0.00317500000000006));
#8568=CARTESIAN_POINT('Origin',(0.0735500000002056,-0.0222000000000067,
0.00817500000000006));
#8569=CARTESIAN_POINT('',(0.0735500000002123,-0.0172000000000067,-0.00182499999999996));
#8570=CARTESIAN_POINT('Origin',(0.0735500000002056,-0.0222000000000067,
-0.00182499999999996));
#8571=CARTESIAN_POINT('',(0.0735500000002123,-0.0172000000000067,-0.00182499999999996));
#8572=CARTESIAN_POINT('Origin',(0.06655,-0.0172,0.02565));
#8573=CARTESIAN_POINT('',(0.04655,-0.0172,-0.001825));
#8574=CARTESIAN_POINT('',(0.04655,-0.0172,-0.009825));
#8575=CARTESIAN_POINT('',(0.04655,-0.0172,0.02565));
#8576=CARTESIAN_POINT('',(0.04655,-0.0172,-0.009825));
#8577=CARTESIAN_POINT('',(0.06655,-0.0172,-0.001825));
#8578=CARTESIAN_POINT('Origin',(0.06655,-0.009975,0.066125));
#8579=CARTESIAN_POINT('',(0.04655,-0.00775,0.066125));
#8580=CARTESIAN_POINT('',(0.06855,-0.00775,0.066125));
#8581=CARTESIAN_POINT('',(0.04655,-0.0122,0.066125));
#8582=CARTESIAN_POINT('',(0.04655,-0.009975,0.066125));
#8583=CARTESIAN_POINT('',(0.068550000000219,-0.0122,0.066125));
#8584=CARTESIAN_POINT('Origin',(0.06655,-0.00275,0.02565));
#8585=CARTESIAN_POINT('',(0.04655,-0.00275,-0.009825));
#8586=CARTESIAN_POINT('',(0.06655,-0.00275,-0.009825));
#8587=CARTESIAN_POINT('',(0.04655,-0.00275,0.061125));
#8588=CARTESIAN_POINT('',(0.04655,-0.00275,0.02565));
#8589=CARTESIAN_POINT('',(0.0685500000002317,-0.00274999999999991,0.061125));
#8590=CARTESIAN_POINT('',(0.05755,-0.00275,0.0218));
#8591=CARTESIAN_POINT('Origin',(0.05755,-0.00275,0.014175));
#8592=CARTESIAN_POINT('',(0.05755,-0.00275,0.04475));
#8593=CARTESIAN_POINT('Origin',(0.05755,-0.00275,0.037125));
#8594=CARTESIAN_POINT('Origin',(0.06655,-0.009975,-0.014825));
#8595=CARTESIAN_POINT('',(0.04655,-0.0122,-0.014825));
#8596=CARTESIAN_POINT('',(0.06855,-0.0122,-0.014825));
#8597=CARTESIAN_POINT('',(0.04655,-0.00775,-0.014825));
#8598=CARTESIAN_POINT('',(0.04655,-0.009975,-0.014825));
#8599=CARTESIAN_POINT('',(0.068550000000225,-0.00774999999999995,-0.014825));
#8600=CARTESIAN_POINT('Origin',(0.06655,-0.009975,-0.0076));
#8601=CARTESIAN_POINT('',(0.06655,-0.009975,-0.003375));
#8602=CARTESIAN_POINT('Origin',(0.06655,-0.009975,-0.0076));
#8603=CARTESIAN_POINT('',(0.04655,-0.009975,-0.003375));
#8604=CARTESIAN_POINT('',(0.06655,-0.009975,-0.003375));
#8605=CARTESIAN_POINT('Origin',(0.04655,-0.009975,-0.0076));
#8606=CARTESIAN_POINT('Origin',(0.06655,-0.0172,0.02565));
#8607=CARTESIAN_POINT('',(0.04655,-0.0172,0.061125));
#8608=CARTESIAN_POINT('',(0.06655,-0.0172,0.061125));
#8609=CARTESIAN_POINT('',(0.04655,-0.0172,0.053125));
#8610=CARTESIAN_POINT('',(0.04655,-0.0172,0.02565));
#8611=CARTESIAN_POINT('',(0.0685500000002123,-0.0172,0.053125));
#8612=CARTESIAN_POINT('Origin',(0.06655,-0.01,0.0589));
#8613=CARTESIAN_POINT('',(0.06655,-0.01,0.063125));
#8614=CARTESIAN_POINT('Origin',(0.06655,-0.01,0.0589));
#8615=CARTESIAN_POINT('',(0.04655,-0.01,0.063125));
#8616=CARTESIAN_POINT('',(0.06655,-0.01,0.063125));
#8617=CARTESIAN_POINT('Origin',(0.04655,-0.01,0.0589));
#8618=CARTESIAN_POINT('Origin',(0.04655,0.,0.02565));
#8619=CARTESIAN_POINT('',(0.04655,-0.0272,0.043125));
#8620=CARTESIAN_POINT('',(0.04655,-0.0272,0.008175));
#8621=CARTESIAN_POINT('',(0.04655,-0.0272,0.02565));
#8622=CARTESIAN_POINT('',(0.04655,-0.0222,0.048125));
#8623=CARTESIAN_POINT('Origin',(0.04655,-0.0222,0.043125));
#8624=CARTESIAN_POINT('Origin',(0.04655,-0.0222,0.053125));
#8625=CARTESIAN_POINT('Origin',(0.04655,-0.0122,0.061125));
#8626=CARTESIAN_POINT('Origin',(0.04655,-0.00775,0.061125));
#8627=CARTESIAN_POINT('Origin',(0.04655,-0.00775,-0.009825));
#8628=CARTESIAN_POINT('Origin',(0.04655,-0.0122,-0.009825));
#8629=CARTESIAN_POINT('',(0.04655,-0.0222,0.003175));
#8630=CARTESIAN_POINT('Origin',(0.04655,-0.0222,-0.001825));
#8631=CARTESIAN_POINT('Origin',(0.04655,-0.0222,0.008175));
#8632=CARTESIAN_POINT('Origin',(0.06655,-0.009975,0.02565));
#8633=CARTESIAN_POINT('Origin',(0.06655,-0.009975,0.02565));
#8634=CARTESIAN_POINT('Origin',(0.06655,-0.0122,0.061125));
#8635=CARTESIAN_POINT('Origin',(0.06655,-0.00775,0.061125));
#8636=CARTESIAN_POINT('Origin',(0.06655,-0.00775,-0.009825));
#8637=CARTESIAN_POINT('Origin',(0.06655,-0.0122,-0.009825));
#8638=CARTESIAN_POINT('Origin',(0.05755,-0.0272,0.02565));
#8639=CARTESIAN_POINT('',(0.0622553825561797,-0.0272,0.043125));
#8640=CARTESIAN_POINT('',(0.0685500000001988,-0.0272,0.0431250000000001));
#8641=CARTESIAN_POINT('',(0.0528446174438203,-0.0272,0.043125));
#8642=CARTESIAN_POINT('Origin',(0.05755,-0.0272,0.037125));
#8643=CARTESIAN_POINT('',(0.05755,-0.0272,0.043125));
#8644=CARTESIAN_POINT('',(0.0528446174438203,-0.0272,0.008175));
#8645=CARTESIAN_POINT('',(0.04655,-0.0272,0.008175));
#8646=CARTESIAN_POINT('',(0.05755,-0.0272,0.0218));
#8647=CARTESIAN_POINT('Origin',(0.05755,-0.0272,0.014175));
#8648=CARTESIAN_POINT('',(0.0622553825561797,-0.0272,0.008175));
#8649=CARTESIAN_POINT('Origin',(0.05755,-0.0272,0.014175));
#8650=CARTESIAN_POINT('',(0.0685500000001989,-0.0272,0.00817500000000003));
#8651=CARTESIAN_POINT('Origin',(0.05755,-0.0022,0.037125));
#8652=CARTESIAN_POINT('',(0.05755,-0.0269285700798444,0.04475));
#8653=CARTESIAN_POINT('',(0.05755,-0.0022,0.04475));
#8654=CARTESIAN_POINT('Ctrl Pts',(0.0528446174438203,-0.0272,0.043125));
#8655=CARTESIAN_POINT('Ctrl Pts',(0.0533814087034594,-0.0272,0.0435459680382359));
#8656=CARTESIAN_POINT('Ctrl Pts',(0.0539899057191737,-0.027146490983882,
0.0439040351600042));
#8657=CARTESIAN_POINT('Ctrl Pts',(0.0555707240629267,-0.0270066019492738,
0.0445577665669935));
#8658=CARTESIAN_POINT('Ctrl Pts',(0.056588612994316,-0.0269285700798444,
0.04475));
#8659=CARTESIAN_POINT('Ctrl Pts',(0.05755,-0.0269285700798444,0.04475));
#8660=CARTESIAN_POINT('Ctrl Pts',(0.05755,-0.0269285700798444,0.04475));
#8661=CARTESIAN_POINT('Ctrl Pts',(0.058511387005684,-0.0269285700798444,
0.04475));
#8662=CARTESIAN_POINT('Ctrl Pts',(0.0595292759370733,-0.0270066019492738,
0.0445577665669935));
#8663=CARTESIAN_POINT('Ctrl Pts',(0.0611100942808263,-0.027146490983882,
0.0439040351600042));
#8664=CARTESIAN_POINT('Ctrl Pts',(0.0617185912965407,-0.0272,0.0435459680382359));
#8665=CARTESIAN_POINT('Ctrl Pts',(0.0622553825561797,-0.0272,0.043125));
#8666=CARTESIAN_POINT('Origin',(0.05755,-0.0022,0.014175));
#8667=CARTESIAN_POINT('',(0.05755,-0.0022,0.0218));
#8668=CARTESIAN_POINT('Ctrl Pts',(0.0622553825561797,-0.0272,0.00817500000000001));
#8669=CARTESIAN_POINT('Ctrl Pts',(0.0617185912965407,-0.0272,0.00775403196176415));
#8670=CARTESIAN_POINT('Ctrl Pts',(0.0611100942808263,-0.027146490983882,
0.00739596483999584));
#8671=CARTESIAN_POINT('Ctrl Pts',(0.0595292759370733,-0.0270066019492738,
0.00674223343300649));
#8672=CARTESIAN_POINT('Ctrl Pts',(0.058511387005684,-0.0269285700798444,
0.00655));
#8673=CARTESIAN_POINT('Ctrl Pts',(0.056588612994316,-0.0269285700798444,
0.00655));
#8674=CARTESIAN_POINT('Ctrl Pts',(0.0555707240629267,-0.0270066019492738,
0.00674223343300649));
#8675=CARTESIAN_POINT('Ctrl Pts',(0.0539899057191737,-0.027146490983882,
0.00739596483999584));
#8676=CARTESIAN_POINT('Ctrl Pts',(0.0533814087034593,-0.0272,0.00775403196176414));
#8677=CARTESIAN_POINT('Ctrl Pts',(0.0528446174438203,-0.0272,0.00817500000000001));
#8678=CARTESIAN_POINT('Origin',(0.05755,-0.0222,0.008175));
#8679=CARTESIAN_POINT('',(0.0685500000002056,-0.0222,0.00317500000000006));
#8680=CARTESIAN_POINT('Origin',(0.05755,-0.0222,-0.001825));
#8681=CARTESIAN_POINT('Origin',(0.05755,-0.0222,0.043125));
#8682=CARTESIAN_POINT('',(0.0685500000002056,-0.0222,0.048125));
#8683=CARTESIAN_POINT('Origin',(0.06655,-0.0222,0.053125));
#8684=CARTESIAN_POINT('',(0.,0.,0.));
#8685=CARTESIAN_POINT('Origin',(0.,2.4492935982947E-19,0.265));
#8686=CARTESIAN_POINT('',(-0.004,-2.44929359829471E-19,0.0015));
#8687=CARTESIAN_POINT('',(0.004,-2.44929359829471E-19,0.00149999999999999));
#8688=CARTESIAN_POINT('Origin',(0.,2.4492935982947E-19,0.0015));
#8689=CARTESIAN_POINT('',(0.004,-2.44929359829471E-19,0.2635));
#8690=CARTESIAN_POINT('',(0.004,-2.44929359829471E-19,0.265));
#8691=CARTESIAN_POINT('',(-0.004,-2.44929359829471E-19,0.2635));
#8692=CARTESIAN_POINT('Origin',(0.,2.4492935982947E-19,0.2635));
#8693=CARTESIAN_POINT('Origin',(0.,2.4492935982947E-19,0.2635));
#8694=CARTESIAN_POINT('Origin',(0.,2.4492935982947E-19,0.0015));
#8695=CARTESIAN_POINT('Origin',(0.,0.,0.265));
#8696=CARTESIAN_POINT('',(-0.0025,-6.12323399573683E-20,0.265));
#8697=CARTESIAN_POINT('Origin',(0.,2.4492935982947E-19,0.265));
#8698=CARTESIAN_POINT('Origin',(0.,0.,0.));
#8699=CARTESIAN_POINT('',(-0.0025,-6.12323399573683E-20,0.));
#8700=CARTESIAN_POINT('Origin',(0.,2.4492935982947E-19,0.));
#8701=CARTESIAN_POINT('Origin',(0.,2.4492935982947E-19,0.0015));
#8702=CARTESIAN_POINT('Origin',(-0.0025,-6.12323399573683E-20,0.0015));
#8703=CARTESIAN_POINT('Origin',(0.,2.4492935982947E-19,0.2635));
#8704=CARTESIAN_POINT('Origin',(-0.0025,-6.12323399573683E-20,0.2635));
#8705=CARTESIAN_POINT('',(0.,0.,0.));
#8706=CARTESIAN_POINT('',(0.,0.,0.));
#8707=CARTESIAN_POINT('Origin',(0.,-0.0109999997541308,0.00699999995096662));
#8708=CARTESIAN_POINT('',(-8.57252759403147E-19,-0.0109999997541408,-0.00700000004903339));
#8709=CARTESIAN_POINT('Origin',(0.,-0.0109999997541408,-4.90433850849834E-11));
#8710=CARTESIAN_POINT('',(-5.26598123633362E-19,-0.0109999997541408,-0.00430000004903338));
#8711=CARTESIAN_POINT('Origin',(0.,-0.0109999997541408,-4.90433850849834E-11));
#8712=CARTESIAN_POINT('Origin',(0.,-0.0107499997597188,-4.90333850849834E-11));
#8713=CARTESIAN_POINT('',(-8.57252759403147E-19,-0.0104999997653167,-0.00700000004903339));
#8714=CARTESIAN_POINT('Origin',(0.,-0.0104999997653167,-4.90433850849834E-11));
#8715=CARTESIAN_POINT('',(-8.57252759403147E-19,-0.0107499997597188,-0.00700000004903339));
#8716=CARTESIAN_POINT('Origin',(0.,-0.0104999997653067,0.00429999995096661));
#8717=CARTESIAN_POINT('',(-5.26598123633362E-19,-0.0104999997653167,-0.00430000004903338));
#8718=CARTESIAN_POINT('Origin',(0.,-0.0104999997653167,-4.90433850849834E-11));
#8719=CARTESIAN_POINT('Origin',(0.,-0.0107499997597188,-4.90333850849834E-11));
#8720=CARTESIAN_POINT('',(-5.26598123633362E-19,-0.0107499997597188,-0.00430000004903338));
#8721=CARTESIAN_POINT('',(0.,0.,0.));
#8722=CARTESIAN_POINT('Origin',(0.,-0.0119,0.));
#8723=CARTESIAN_POINT('',(0.,-0.01180000000001,-0.00650000000001));
#8724=CARTESIAN_POINT('',(-7.96020419447004E-19,-0.01180000000001,0.00650000000001));
#8725=CARTESIAN_POINT('Origin',(0.,-0.01180000000001,0.));
#8726=CARTESIAN_POINT('',(-8.20513355429951E-19,-0.01200000000001,0.00670000000001));
#8727=CARTESIAN_POINT('',(-8.08266887437253E-19,-0.0119,0.0066));
#8728=CARTESIAN_POINT('Origin',(0.,-0.01200000000001,0.));
#8729=CARTESIAN_POINT('Origin',(0.,-0.01180000000001,0.));
#8730=CARTESIAN_POINT('Origin',(0.,-0.012,0.0075));
#8731=CARTESIAN_POINT('',(8.93992163377568E-19,-0.012,0.0073));
#8732=CARTESIAN_POINT('Origin',(0.,-0.01200000000001,0.));
#8733=CARTESIAN_POINT('Origin',(0.,-0.0115000000819564,0.));
#8734=CARTESIAN_POINT('',(-7.9602041944578E-19,-0.0110000001639228,-0.0065));
#8735=CARTESIAN_POINT('',(-7.9602041944578E-19,-0.0115000000819564,-0.0065));
#8736=CARTESIAN_POINT('Origin',(0.,-0.0110000001639228,0.));
#8737=CARTESIAN_POINT('Origin',(0.,-0.0119,0.));
#8738=CARTESIAN_POINT('',(0.,-0.01180000000001,-0.00750000000001));
#8739=CARTESIAN_POINT('',(9.18485099360515E-19,-0.0118,0.0075));
#8740=CARTESIAN_POINT('Origin',(0.,-0.01180000000001,0.));
#8741=CARTESIAN_POINT('',(9.06238631369041E-19,-0.0119,0.0074));
#8742=CARTESIAN_POINT('Origin',(0.,-0.01180000000001,0.));
#8743=CARTESIAN_POINT('Origin',(0.,-0.010375,0.));
#8744=CARTESIAN_POINT('',(-9.18485099360515E-19,-0.00875000000001,-0.0075));
#8745=CARTESIAN_POINT('Origin',(0.,-0.00875000000001,0.));
#8746=CARTESIAN_POINT('',(-9.18485099360515E-19,-0.010375,-0.0075));
#8747=CARTESIAN_POINT('Origin',(0.,0.0119,0.));
#8748=CARTESIAN_POINT('',(0.,0.01180000000001,-0.00650000000001));
#8749=CARTESIAN_POINT('',(7.96020419447004E-19,0.01180000000001,0.00650000000001));
#8750=CARTESIAN_POINT('Origin',(0.,0.01180000000001,0.));
#8751=CARTESIAN_POINT('',(8.20513355429951E-19,0.01200000000001,0.00670000000001));
#8752=CARTESIAN_POINT('',(8.08266887437253E-19,0.0119,0.0066));
#8753=CARTESIAN_POINT('Origin',(0.,0.01200000000001,0.));
#8754=CARTESIAN_POINT('Origin',(0.,0.01180000000001,0.));
#8755=CARTESIAN_POINT('Origin',(0.,0.012,0.0065));
#8756=CARTESIAN_POINT('',(-8.93992163377568E-19,0.012,0.0073));
#8757=CARTESIAN_POINT('Origin',(0.,0.01200000000001,0.));
#8758=CARTESIAN_POINT('Origin',(0.,0.0115000000819564,0.));
#8759=CARTESIAN_POINT('',(-7.9602041944578E-19,0.0110000001639228,-0.0065));
#8760=CARTESIAN_POINT('Origin',(0.,0.0110000001639228,0.));
#8761=CARTESIAN_POINT('',(-7.9602041944578E-19,0.0115000000819564,-0.0065));
#8762=CARTESIAN_POINT('Origin',(0.,0.0119,0.));
#8763=CARTESIAN_POINT('',(0.,0.01180000000001,-0.00750000000001));
#8764=CARTESIAN_POINT('',(-9.18485099360515E-19,0.0118,0.0075));
#8765=CARTESIAN_POINT('Origin',(0.,0.01180000000001,0.));
#8766=CARTESIAN_POINT('',(-9.06238631369041E-19,0.0119,0.0074));
#8767=CARTESIAN_POINT('Origin',(0.,0.01180000000001,0.));
#8768=CARTESIAN_POINT('Origin',(0.,0.010375,0.));
#8769=CARTESIAN_POINT('',(-9.18485099360515E-19,0.00875000000001,-0.0075));
#8770=CARTESIAN_POINT('',(-9.18485099360515E-19,0.010375,-0.0075));
#8771=CARTESIAN_POINT('Origin',(0.,0.00875000000001,0.));
#8772=CARTESIAN_POINT('Origin',(0.,0.0110000001639128,0.00700000010430813));
#8773=CARTESIAN_POINT('',(-8.57252772177209E-19,0.0110000001639228,-0.00700000010430813));
#8774=CARTESIAN_POINT('Origin',(0.,0.0110000001639228,0.));
#8775=CARTESIAN_POINT('Origin',(0.,0.0107500001601875,0.));
#8776=CARTESIAN_POINT('',(-8.57252772177209E-19,0.0105000001564722,-0.00700000010430813));
#8777=CARTESIAN_POINT('Origin',(0.,0.0105000001564722,0.));
#8778=CARTESIAN_POINT('',(-8.57252772177209E-19,0.0107500001601875,-0.00700000010430813));
#8779=CARTESIAN_POINT('Origin',(0.,0.0105000001564622,0.0063));
#8780=CARTESIAN_POINT('',(-7.71527483462833E-19,0.0105000001564722,-0.0063));
#8781=CARTESIAN_POINT('Origin',(0.,0.0105000001564722,0.));
#8782=CARTESIAN_POINT('Origin',(0.,0.0093500000782311,0.));
#8783=CARTESIAN_POINT('',(-7.71527483462833E-19,0.00820000000001,-0.0063));
#8784=CARTESIAN_POINT('Origin',(0.,0.00820000000001,0.));
#8785=CARTESIAN_POINT('',(-7.71527483462833E-19,0.0093500000782311,-0.0063));
#8786=CARTESIAN_POINT('Origin',(0.,0.00695,0.));
#8787=CARTESIAN_POINT('',(-7.2254161149716E-19,0.00570000000001131,-0.00590000000000181));
#8788=CARTESIAN_POINT('Origin',(0.,0.00570000000001,0.));
#8789=CARTESIAN_POINT('',(-7.47034547479885E-19,0.00695,-0.0061));
#8790=CARTESIAN_POINT('Origin',(0.,0.,0.));
#8791=CARTESIAN_POINT('',(-7.22541611496938E-19,-0.00570000000001,-0.0059));
#8792=CARTESIAN_POINT('Origin',(0.,-0.00570000000001,0.));
#8793=CARTESIAN_POINT('',(-7.22541611496938E-19,0.,-0.0059));
#8794=CARTESIAN_POINT('Origin',(0.,-0.00695,0.));
#8795=CARTESIAN_POINT('',(7.71527483463054E-19,-0.00820000000001131,-0.00630000000000181));
#8796=CARTESIAN_POINT('',(7.47034547479885E-19,-0.00695,-0.0061));
#8797=CARTESIAN_POINT('Origin',(0.,-0.00820000000001,0.));
#8798=CARTESIAN_POINT('Origin',(0.,-0.0093500000782311,0.));
#8799=CARTESIAN_POINT('',(-7.71527483462833E-19,-0.0105000001564722,-0.0063));
#8800=CARTESIAN_POINT('Origin',(0.,-0.0105000001564722,0.));
#8801=CARTESIAN_POINT('',(-7.71527483462833E-19,-0.0093500000782311,-0.0063));
#8802=CARTESIAN_POINT('Origin',(0.,-0.0105000001564622,0.00700000010430813));
#8803=CARTESIAN_POINT('',(-8.57252772177209E-19,-0.0105000001564722,-0.00700000010430813));
#8804=CARTESIAN_POINT('Origin',(0.,-0.0105000001564722,0.));
#8805=CARTESIAN_POINT('Origin',(0.,-0.0107500001601875,0.));
#8806=CARTESIAN_POINT('',(-8.57252772177209E-19,-0.0110000001639228,-0.00700000010430813));
#8807=CARTESIAN_POINT('Origin',(0.,-0.0110000001639228,0.));
#8808=CARTESIAN_POINT('',(-8.57252772177209E-19,-0.0107500001601875,-0.00700000010430813));
#8809=CARTESIAN_POINT('Origin',(0.,-0.0110000001639128,0.0065));
#8810=CARTESIAN_POINT('Origin',(0.,-0.00875,0.00715));
#8811=CARTESIAN_POINT('',(-8.75622461390357E-19,-0.00875000000001,-0.00715));
#8812=CARTESIAN_POINT('Origin',(0.,-0.00875000000001,0.));
#8813=CARTESIAN_POINT('Origin',(0.,-0.0082,0.));
#8814=CARTESIAN_POINT('',(-8.75622461390357E-19,-0.00765000000001,-0.00715));
#8815=CARTESIAN_POINT('Origin',(0.,-0.00765000000001,0.));
#8816=CARTESIAN_POINT('',(-8.75622461390357E-19,-0.0082,-0.00715));
#8817=CARTESIAN_POINT('Origin',(0.,-0.00765,0.0075));
#8818=CARTESIAN_POINT('',(-9.18485099360515E-19,-0.00765000000001,-0.0075));
#8819=CARTESIAN_POINT('Origin',(0.,-0.00765000000001,0.));
#8820=CARTESIAN_POINT('Origin',(0.,0.,0.));
#8821=CARTESIAN_POINT('',(-9.18485099360515E-19,0.00765000000001,-0.0075));
#8822=CARTESIAN_POINT('Origin',(0.,0.00765000000001,0.));
#8823=CARTESIAN_POINT('',(-9.18485099360515E-19,0.,-0.0075));
#8824=CARTESIAN_POINT('Origin',(0.,0.00765,0.00715));
#8825=CARTESIAN_POINT('',(-8.75622461390357E-19,0.00765000000001,-0.00715));
#8826=CARTESIAN_POINT('Origin',(0.,0.00765000000001,0.));
#8827=CARTESIAN_POINT('Origin',(0.,0.0082,0.));
#8828=CARTESIAN_POINT('',(-8.75622461390357E-19,0.00875000000001,-0.00715));
#8829=CARTESIAN_POINT('Origin',(0.,0.00875000000001,0.));
#8830=CARTESIAN_POINT('',(-8.75622461390357E-19,0.0082,-0.00715));
#8831=CARTESIAN_POINT('Origin',(0.,0.00875,0.0075));
#8832=CARTESIAN_POINT('',(0.,0.,0.));
#8833=CARTESIAN_POINT('Origin',(0.,-0.0116999997384846,0.0065));
#8834=CARTESIAN_POINT('',(-7.9602041944578E-19,-0.0116999997384946,-0.0065));
#8835=CARTESIAN_POINT('Origin',(0.,-0.0116999997384946,0.));
#8836=CARTESIAN_POINT('',(-5.87830450451699E-19,-0.0116999997384846,-0.00479999989271167));
#8837=CARTESIAN_POINT('Origin',(0.,-0.0116999997384946,0.));
#8838=CARTESIAN_POINT('Origin',(0.,-0.0113499997351319,0.));
#8839=CARTESIAN_POINT('',(-7.9602041944578E-19,-0.0109999997317891,-0.0065));
#8840=CARTESIAN_POINT('Origin',(0.,-0.0109999997317891,0.));
#8841=CARTESIAN_POINT('',(-7.9602041944578E-19,-0.0113499997351319,-0.0065));
#8842=CARTESIAN_POINT('Origin',(0.,-0.0109999997317791,0.00455));
#8843=CARTESIAN_POINT('',(-5.57214293612046E-19,-0.0109999997317791,-0.00455));
#8844=CARTESIAN_POINT('Origin',(0.,-0.0109999997317891,0.));
#8845=CARTESIAN_POINT('Origin',(0.,-0.0112499997317791,0.));
#8846=CARTESIAN_POINT('',(-4.95981953654678E-19,-0.0114999997317791,-0.00405));
#8847=CARTESIAN_POINT('Origin',(0.,-0.0114999997317891,0.));
#8848=CARTESIAN_POINT('',(-5.26598123633362E-19,-0.0112499997317791,-0.0043));
#8849=CARTESIAN_POINT('Origin',(0.,-0.0117499997317791,0.));
#8850=CARTESIAN_POINT('',(-4.95981953654678E-19,-0.0119999997317891,-0.00405));
#8851=CARTESIAN_POINT('Origin',(0.,-0.0119999997317891,0.));
#8852=CARTESIAN_POINT('',(-4.95981953654678E-19,-0.0117499997317791,-0.00405));
#8853=CARTESIAN_POINT('Origin',(0.,-0.0119999997317791,0.00449999989941716));
#8854=CARTESIAN_POINT('',(-5.51091047298466E-19,-0.0119999997317791,-0.00449999989941718));
#8855=CARTESIAN_POINT('Origin',(0.,-0.0119999997317891,0.));
#8856=CARTESIAN_POINT('Origin',(0.,-0.0118499997351319,0.));
#8857=CARTESIAN_POINT('',(-5.69460748875079E-19,-0.0118499997351319,-0.0046499998960644));
#8858=CARTESIAN_POINT('',(0.,0.,0.));
#8859=CARTESIAN_POINT('Origin',(0.,0.0109999997541308,0.00699999995096662));
#8860=CARTESIAN_POINT('',(-8.57252759403147E-19,0.0109999997541408,-0.00700000004903339));
#8861=CARTESIAN_POINT('Origin',(0.,0.0109999997541408,-4.90433850849834E-11));
#8862=CARTESIAN_POINT('',(-5.26598123633362E-19,0.0109999997541408,-0.00430000004903338));
#8863=CARTESIAN_POINT('Origin',(0.,0.0109999997541408,-4.90433850849834E-11));
#8864=CARTESIAN_POINT('Origin',(0.,0.0107499997597188,-4.90333850849834E-11));
#8865=CARTESIAN_POINT('',(-8.57252759403147E-19,0.0104999997653167,-0.00700000004903339));
#8866=CARTESIAN_POINT('',(-8.57252759403147E-19,0.0107499997597188,-0.00700000004903339));
#8867=CARTESIAN_POINT('Origin',(0.,0.0104999997653167,-4.90433850849834E-11));
#8868=CARTESIAN_POINT('Origin',(0.,0.0104999997653067,0.00429999995096661));
#8869=CARTESIAN_POINT('',(-5.26598123633362E-19,0.0104999997653167,-0.00430000004903338));
#8870=CARTESIAN_POINT('Origin',(0.,0.0104999997653167,-4.90433850849834E-11));
#8871=CARTESIAN_POINT('Origin',(0.,0.0107499997597188,-4.90333850849834E-11));
#8872=CARTESIAN_POINT('',(-5.26598123633362E-19,0.0107499997597188,-0.00430000004903338));
#8873=CARTESIAN_POINT('',(0.,0.,0.));
#8874=CARTESIAN_POINT('Origin',(0.,0.0116999997384846,0.0065));
#8875=CARTESIAN_POINT('',(-7.9602041944578E-19,0.0116999997384946,-0.0065));
#8876=CARTESIAN_POINT('Origin',(0.,0.0116999997384946,0.));
#8877=CARTESIAN_POINT('',(5.87830450451699E-19,0.0116999997384846,-0.00479999989271167));
#8878=CARTESIAN_POINT('Origin',(0.,0.0116999997384946,0.));
#8879=CARTESIAN_POINT('Origin',(0.,0.0113499997351319,0.));
#8880=CARTESIAN_POINT('',(-7.9602041944578E-19,0.0109999997317891,-0.0065));
#8881=CARTESIAN_POINT('',(-7.9602041944578E-19,0.0113499997351319,-0.0065));
#8882=CARTESIAN_POINT('Origin',(0.,0.0109999997317891,0.));
#8883=CARTESIAN_POINT('Origin',(0.,0.0109999997317791,0.00455));
#8884=CARTESIAN_POINT('',(5.57214293612046E-19,0.0109999997317791,-0.00455));
#8885=CARTESIAN_POINT('Origin',(0.,0.0109999997317891,0.));
#8886=CARTESIAN_POINT('Origin',(0.,0.0112499997317791,0.));
#8887=CARTESIAN_POINT('',(4.95981953654678E-19,0.0114999997317791,-0.00405));
#8888=CARTESIAN_POINT('Origin',(0.,0.0114999997317891,0.));
#8889=CARTESIAN_POINT('',(5.26598123633362E-19,0.0112499997317791,-0.0043));
#8890=CARTESIAN_POINT('Origin',(0.,0.0117499997317791,0.));
#8891=CARTESIAN_POINT('',(-4.95981953654678E-19,0.0119999997317891,-0.00405));
#8892=CARTESIAN_POINT('',(-4.95981953654678E-19,0.0117499997317791,-0.00405));
#8893=CARTESIAN_POINT('Origin',(0.,0.0119999997317891,0.));
#8894=CARTESIAN_POINT('Origin',(0.,0.0119999997317791,0.00449999989941716));
#8895=CARTESIAN_POINT('',(5.51091047298466E-19,0.0119999997317791,-0.00449999989941718));
#8896=CARTESIAN_POINT('Origin',(0.,0.0119999997317891,0.));
#8897=CARTESIAN_POINT('Origin',(0.,0.0118499997351319,0.));
#8898=CARTESIAN_POINT('',(5.69460748875079E-19,0.0118499997351319,-0.0046499998960644));
#8899=CARTESIAN_POINT('',(-0.00162514689746462,0.160028668339065,0.190074877802291));
#8900=CARTESIAN_POINT('',(-0.00162514689746462,0.160028668339065,0.190074877802291));
#8901=CARTESIAN_POINT('',(-0.00162514689746462,0.160028668339065,0.190074877802291));
#8902=CARTESIAN_POINT('',(-0.00162514689746462,0.160028668339065,0.190074877802291));
#8903=CARTESIAN_POINT('',(-0.00162514689746462,0.160028668339065,0.190074877802291));
#8904=CARTESIAN_POINT('',(0.0559239276780895,0.175232171734558,0.152949877802291));
#8905=CARTESIAN_POINT('',(0.120084284659387,0.175239760780052,0.152861959395576));
#8906=CARTESIAN_POINT('',(0.187823927433681,0.175240201301577,0.152949877802291));
#8907=CARTESIAN_POINT('',(0.,0.,0.));
#8908=CARTESIAN_POINT('',(0.254374534550176,0.165269252629273,0.145349877802291));
#8909=CARTESIAN_POINT('',(0.245383509507527,0.0178392517997215,0.167124877802291));
#8910=CARTESIAN_POINT('',(0.245367377322084,0.282839251308684,0.190074877802291));
#8911=CARTESIAN_POINT('',(-0.0016316401699145,0.266692282029197,0.190074877802291));
#8912=CARTESIAN_POINT('',(0.254374536072079,0.165244252629318,0.211849877802292));
#8913=CARTESIAN_POINT('',(-0.00161550798447187,0.00169228252022999,0.167124877802291));
#8914=CARTESIAN_POINT('',(-0.182343169146509,-0.000311100616136057,0.226019166440506));
#8915=CARTESIAN_POINT('',(0.267674662399915,-0.015479037621645,0.270356248033791));
#8916=CARTESIAN_POINT('',(0.291674662355448,-0.0154775765935299,0.270356248033792));
#8917=CARTESIAN_POINT('',(0.292574661830748,-0.0154775218050085,0.204156248033792));
#8918=CARTESIAN_POINT('',(0.268574661875219,-0.0154789828331232,0.204156248033792));
#8919=CARTESIAN_POINT('',(0.426092911419626,0.319783473186682,0.248969166440507));
#8920=CARTESIAN_POINT('',(0.426092911419626,0.319783473186683,0.226019166440507));
#8921=UNCERTAINTY_MEASURE_WITH_UNIT(LENGTH_MEASURE(1.E-5),#8945,
'DISTANCE_ACCURACY_VALUE',
'Maximum model space distance between geometric entities at asserted c
onnectivities');
#8922=UNCERTAINTY_MEASURE_WITH_UNIT(LENGTH_MEASURE(1.E-5),#8945,
'DISTANCE_ACCURACY_VALUE',
'Maximum model space distance between geometric entities at asserted c
onnectivities');
#8923=UNCERTAINTY_MEASURE_WITH_UNIT(LENGTH_MEASURE(1.E-5),#8945,
'DISTANCE_ACCURACY_VALUE',
'Maximum model space distance between geometric entities at asserted c
onnectivities');
#8924=UNCERTAINTY_MEASURE_WITH_UNIT(LENGTH_MEASURE(1.E-5),#8945,
'DISTANCE_ACCURACY_VALUE',
'Maximum model space distance between geometric entities at asserted c
onnectivities');
#8925=UNCERTAINTY_MEASURE_WITH_UNIT(LENGTH_MEASURE(1.E-5),#8945,
'DISTANCE_ACCURACY_VALUE',
'Maximum model space distance between geometric entities at asserted c
onnectivities');
#8926=UNCERTAINTY_MEASURE_WITH_UNIT(LENGTH_MEASURE(1.E-5),#8945,
'DISTANCE_ACCURACY_VALUE',
'Maximum model space distance between geometric entities at asserted c
onnectivities');
#8927=UNCERTAINTY_MEASURE_WITH_UNIT(LENGTH_MEASURE(1.E-5),#8945,
'DISTANCE_ACCURACY_VALUE',
'Maximum model space distance between geometric entities at asserted c
onnectivities');
#8928=UNCERTAINTY_MEASURE_WITH_UNIT(LENGTH_MEASURE(1.E-5),#8945,
'DISTANCE_ACCURACY_VALUE',
'Maximum model space distance between geometric entities at asserted c
onnectivities');
#8929=UNCERTAINTY_MEASURE_WITH_UNIT(LENGTH_MEASURE(1.E-5),#8945,
'DISTANCE_ACCURACY_VALUE',
'Maximum model space distance between geometric entities at asserted c
onnectivities');
#8930=UNCERTAINTY_MEASURE_WITH_UNIT(LENGTH_MEASURE(1.E-5),#8945,
'DISTANCE_ACCURACY_VALUE',
'Maximum model space distance between geometric entities at asserted c
onnectivities');
#8931=UNCERTAINTY_MEASURE_WITH_UNIT(LENGTH_MEASURE(1.E-5),#8945,
'DISTANCE_ACCURACY_VALUE',
'Maximum model space distance between geometric entities at asserted c
onnectivities');
#8932=UNCERTAINTY_MEASURE_WITH_UNIT(LENGTH_MEASURE(1.E-5),#8945,
'DISTANCE_ACCURACY_VALUE',
'Maximum model space distance between geometric entities at asserted c
onnectivities');
#8933=(
GEOMETRIC_REPRESENTATION_CONTEXT(3)
GLOBAL_UNCERTAINTY_ASSIGNED_CONTEXT((#8921))
GLOBAL_UNIT_ASSIGNED_CONTEXT((#8945,#8946,#8947))
REPRESENTATION_CONTEXT('','3D')
);
#8934=(
GEOMETRIC_REPRESENTATION_CONTEXT(3)
GLOBAL_UNCERTAINTY_ASSIGNED_CONTEXT((#8922))
GLOBAL_UNIT_ASSIGNED_CONTEXT((#8945,#8946,#8947))
REPRESENTATION_CONTEXT('','3D')
);
#8935=(
GEOMETRIC_REPRESENTATION_CONTEXT(3)
GLOBAL_UNCERTAINTY_ASSIGNED_CONTEXT((#8923))
GLOBAL_UNIT_ASSIGNED_CONTEXT((#8945,#8946,#8947))
REPRESENTATION_CONTEXT('','3D')
);
#8936=(
GEOMETRIC_REPRESENTATION_CONTEXT(3)
GLOBAL_UNCERTAINTY_ASSIGNED_CONTEXT((#8924))
GLOBAL_UNIT_ASSIGNED_CONTEXT((#8945,#8946,#8947))
REPRESENTATION_CONTEXT('','3D')
);
#8937=(
GEOMETRIC_REPRESENTATION_CONTEXT(3)
GLOBAL_UNCERTAINTY_ASSIGNED_CONTEXT((#8925))
GLOBAL_UNIT_ASSIGNED_CONTEXT((#8945,#8946,#8947))
REPRESENTATION_CONTEXT('','3D')
);
#8938=(
GEOMETRIC_REPRESENTATION_CONTEXT(3)
GLOBAL_UNCERTAINTY_ASSIGNED_CONTEXT((#8926))
GLOBAL_UNIT_ASSIGNED_CONTEXT((#8945,#8946,#8947))
REPRESENTATION_CONTEXT('','3D')
);
#8939=(
GEOMETRIC_REPRESENTATION_CONTEXT(3)
GLOBAL_UNCERTAINTY_ASSIGNED_CONTEXT((#8927))
GLOBAL_UNIT_ASSIGNED_CONTEXT((#8945,#8946,#8947))
REPRESENTATION_CONTEXT('','3D')
);
#8940=(
GEOMETRIC_REPRESENTATION_CONTEXT(3)
GLOBAL_UNCERTAINTY_ASSIGNED_CONTEXT((#8928))
GLOBAL_UNIT_ASSIGNED_CONTEXT((#8945,#8946,#8947))
REPRESENTATION_CONTEXT('','3D')
);
#8941=(
GEOMETRIC_REPRESENTATION_CONTEXT(3)
GLOBAL_UNCERTAINTY_ASSIGNED_CONTEXT((#8929))
GLOBAL_UNIT_ASSIGNED_CONTEXT((#8945,#8946,#8947))
REPRESENTATION_CONTEXT('','3D')
);
#8942=(
GEOMETRIC_REPRESENTATION_CONTEXT(3)
GLOBAL_UNCERTAINTY_ASSIGNED_CONTEXT((#8930))
GLOBAL_UNIT_ASSIGNED_CONTEXT((#8945,#8946,#8947))
REPRESENTATION_CONTEXT('','3D')
);
#8943=(
GEOMETRIC_REPRESENTATION_CONTEXT(3)
GLOBAL_UNCERTAINTY_ASSIGNED_CONTEXT((#8931))
GLOBAL_UNIT_ASSIGNED_CONTEXT((#8945,#8946,#8947))
REPRESENTATION_CONTEXT('','3D')
);
#8944=(
GEOMETRIC_REPRESENTATION_CONTEXT(3)
GLOBAL_UNCERTAINTY_ASSIGNED_CONTEXT((#8932))
GLOBAL_UNIT_ASSIGNED_CONTEXT((#8945,#8946,#8947))
REPRESENTATION_CONTEXT('','3D')
);
#8945=(
LENGTH_UNIT()
NAMED_UNIT(*)
SI_UNIT($,.METRE.)
);
#8946=(
NAMED_UNIT(*)
PLANE_ANGLE_UNIT()
SI_UNIT($,.RADIAN.)
);
#8947=(
NAMED_UNIT(*)
SI_UNIT($,.STERADIAN.)
SOLID_ANGLE_UNIT()
);
#8948=SHAPE_DEFINITION_REPRESENTATION(#8959,#8992);
#8949=SHAPE_DEFINITION_REPRESENTATION(#8960,#8993);
#8950=SHAPE_DEFINITION_REPRESENTATION(#8961,#8994);
#8951=SHAPE_DEFINITION_REPRESENTATION(#8962,#8995);
#8952=SHAPE_DEFINITION_REPRESENTATION(#8963,#8996);
#8953=SHAPE_DEFINITION_REPRESENTATION(#8964,#8997);
#8954=SHAPE_DEFINITION_REPRESENTATION(#8965,#8998);
#8955=SHAPE_DEFINITION_REPRESENTATION(#8966,#8999);
#8956=SHAPE_DEFINITION_REPRESENTATION(#8967,#9000);
#8957=SHAPE_DEFINITION_REPRESENTATION(#8968,#9001);
#8958=SHAPE_DEFINITION_REPRESENTATION(#8969,#9002);
#8959=PRODUCT_DEFINITION_SHAPE('',$,#9004);
#8960=PRODUCT_DEFINITION_SHAPE('',$,#9005);
#8961=PRODUCT_DEFINITION_SHAPE('',$,#9006);
#8962=PRODUCT_DEFINITION_SHAPE('',$,#9007);
#8963=PRODUCT_DEFINITION_SHAPE('',$,#9008);
#8964=PRODUCT_DEFINITION_SHAPE('',$,#9009);
#8965=PRODUCT_DEFINITION_SHAPE('',$,#9010);
#8966=PRODUCT_DEFINITION_SHAPE('',$,#9011);
#8967=PRODUCT_DEFINITION_SHAPE('',$,#9012);
#8968=PRODUCT_DEFINITION_SHAPE('',$,#9013);
#8969=PRODUCT_DEFINITION_SHAPE('',$,#9014);
#8970=PRODUCT_DEFINITION_SHAPE($,$,#77);
#8971=PRODUCT_DEFINITION_SHAPE($,$,#78);
#8972=PRODUCT_DEFINITION_SHAPE($,$,#79);
#8973=PRODUCT_DEFINITION_SHAPE($,$,#80);
#8974=PRODUCT_DEFINITION_SHAPE($,$,#81);
#8975=PRODUCT_DEFINITION_SHAPE($,$,#82);
#8976=PRODUCT_DEFINITION_SHAPE($,$,#83);
#8977=PRODUCT_DEFINITION_SHAPE($,$,#84);
#8978=PRODUCT_DEFINITION_SHAPE($,$,#85);
#8979=PRODUCT_DEFINITION_SHAPE($,$,#86);
#8980=PRODUCT_DEFINITION_SHAPE($,$,#87);
#8981=PRODUCT_DEFINITION_SHAPE($,$,#88);
#8982=PRODUCT_DEFINITION_SHAPE($,$,#89);
#8983=PRODUCT_DEFINITION_SHAPE($,$,#90);
#8984=PRODUCT_DEFINITION_SHAPE($,$,#91);
#8985=PRODUCT_DEFINITION_SHAPE($,$,#92);
#8986=PRODUCT_DEFINITION_SHAPE($,$,#93);
#8987=PRODUCT_DEFINITION_SHAPE($,$,#94);
#8988=PRODUCT_DEFINITION_SHAPE($,$,#95);
#8989=PRODUCT_DEFINITION_SHAPE($,$,#96);
#8990=PRODUCT_DEFINITION_SHAPE($,$,#97);
#8991=PRODUCT_DEFINITION_SHAPE($,$,#98);
#8992=SHAPE_REPRESENTATION('',(#5259,#5800,#5801,#5802,#5803,#5804,#5805,
#5806,#5807,#5808,#5809,#5810,#5811,#5812,#5813,#5814,#5815,#5816),#8933);
#8993=SHAPE_REPRESENTATION('',(#5260),#8934);
#8994=SHAPE_REPRESENTATION('',(#5308),#8935);
#8995=SHAPE_REPRESENTATION('',(#5623),#8936);
#8996=SHAPE_REPRESENTATION('',(#5671),#8937);
#8997=SHAPE_REPRESENTATION('',(#5685,#5795,#5796,#5797,#5798,#5799),#8938);
#8998=SHAPE_REPRESENTATION('',(#5686),#8939);
#8999=SHAPE_REPRESENTATION('',(#5695),#8940);
#9000=SHAPE_REPRESENTATION('',(#5756),#8941);
#9001=SHAPE_REPRESENTATION('',(#5771),#8942);
#9002=SHAPE_REPRESENTATION('',(#5780),#8943);
#9003=PRODUCT_DEFINITION_CONTEXT('part definition',#9038,'design');
#9004=PRODUCT_DEFINITION('2026-10-24-22-39-37-629',
'MAT-066',#9015,#9003);
#9005=PRODUCT_DEFINITION('End Cap Left','End Cap Left',#9016,#9003);
#9006=PRODUCT_DEFINITION('Motor Mount','Motor Mount',#9017,#9003);
#9007=PRODUCT_DEFINITION('End Cap Right','End Cap Right',#9018,#9003);
#9008=PRODUCT_DEFINITION('Z Axis Rod','Z Axis Rod',#9019,#9003);
#9009=PRODUCT_DEFINITION('Bearing Assembly','Bearing Assembly 1',#9020,
#9003);
#9010=PRODUCT_DEFINITION('Bearing Sleeve','Bearing Sleeve',#9021,#9003);
#9011=PRODUCT_DEFINITION('Ball Bushing','Ball Bushing',#9022,#9003);
#9012=PRODUCT_DEFINITION('Bearing Retainer','Bearing Retainer 1',#9023,
#9003);
#9013=PRODUCT_DEFINITION('Gantry Support Bracket',
'Gantry Support Bracket',#9024,#9003);
#9014=PRODUCT_DEFINITION('Gantry Carriage Bracket',
'Gantry Carriage Bracket',#9025,#9003);
#9015=PRODUCT_DEFINITION_FORMATION('',$,#9040);
#9016=PRODUCT_DEFINITION_FORMATION('',$,#9041);
#9017=PRODUCT_DEFINITION_FORMATION('',$,#9042);
#9018=PRODUCT_DEFINITION_FORMATION('',$,#9043);
#9019=PRODUCT_DEFINITION_FORMATION('',$,#9044);
#9020=PRODUCT_DEFINITION_FORMATION('',$,#9045);
#9021=PRODUCT_DEFINITION_FORMATION('',$,#9046);
#9022=PRODUCT_DEFINITION_FORMATION('',$,#9047);
#9023=PRODUCT_DEFINITION_FORMATION('',$,#9048);
#9024=PRODUCT_DEFINITION_FORMATION('',$,#9049);
#9025=PRODUCT_DEFINITION_FORMATION('',$,#9050);
#9026=PRODUCT_RELATED_PRODUCT_CATEGORY('MAT-066',
'MAT-066',(#9040));
#9027=PRODUCT_RELATED_PRODUCT_CATEGORY('End Cap Left','End Cap Left',(#9041));
#9028=PRODUCT_RELATED_PRODUCT_CATEGORY('Motor Mount','Motor Mount',(#9042));
#9029=PRODUCT_RELATED_PRODUCT_CATEGORY('End Cap Right','End Cap Right',
(#9043));
#9030=PRODUCT_RELATED_PRODUCT_CATEGORY('Z Axis Rod','Z Axis Rod',(#9044));
#9031=PRODUCT_RELATED_PRODUCT_CATEGORY('Bearing Assembly 1',
'Bearing Assembly 1',(#9045));
#9032=PRODUCT_RELATED_PRODUCT_CATEGORY('Bearing Sleeve',
'Bearing Sleeve',(#9046));
#9033=PRODUCT_RELATED_PRODUCT_CATEGORY('Ball Bushing','Ball Bushing',(#9047));
#9034=PRODUCT_RELATED_PRODUCT_CATEGORY('Bearing Retainer 1',
'Bearing Retainer 1',(#9048));
#9035=PRODUCT_RELATED_PRODUCT_CATEGORY('Gantry Support Bracket',
'Gantry Support Bracket',(#9049));
#9036=PRODUCT_RELATED_PRODUCT_CATEGORY('Gantry Carriage Bracket',
'Gantry Carriage Bracket',(#9050));
#9037=APPLICATION_PROTOCOL_DEFINITION('international standard',
'ap242_managed_model_based_3d_engineering',2011,#9038);
#9038=APPLICATION_CONTEXT('Managed model based 3d engineering');
#9039=PRODUCT_CONTEXT('part definition',#9038,'mechanical');
#9040=PRODUCT('2026-10-24-22-39-37-629','MAT-066',
'LEGAL AND USAGE DISCLAIMER: this Data/Model is provided \X2\201C\X0\A
S IS\X2\201D\X0\ for informational and representational only. It is a 
geometric approximation and is NOT engineered, certified, or guarantee
d for dimensional accuracy, exact tolerances, or production-level prec
ision. Vendor disclaims all implied warranties including fitness for a
 particular purpose. DO NOT USE FOR DIRECT PHYSICAL MANUFACTURING, AUT
OMATED PRODUCTION, OR SAFETY-CRITICAL SYSTEMS without independent engi
neering verification and resolution of any design discrepancies.',(#9039));
#9041=PRODUCT('End Cap Left','End Cap Left',
'LEGAL AND USAGE DISCLAIMER: this Data/Model is provided \X2\201C\X0\A
S IS\X2\201D\X0\ for informational and representational only. It is a 
geometric approximation and is NOT engineered, certified, or guarantee
d for dimensional accuracy, exact tolerances, or production-level prec
ision. Vendor disclaims all implied warranties including fitness for a
 particular purpose. DO NOT USE FOR DIRECT PHYSICAL MANUFACTURING, AUT
OMATED PRODUCTION, OR SAFETY-CRITICAL SYSTEMS without independent engi
neering verification and resolution of any design discrepancies.',(#9039));
#9042=PRODUCT('Motor Mount','Motor Mount',
'LEGAL AND USAGE DISCLAIMER: this Data/Model is provided \X2\201C\X0\A
S IS\X2\201D\X0\ for informational and representational only. It is a 
geometric approximation and is NOT engineered, certified, or guarantee
d for dimensional accuracy, exact tolerances, or production-level prec
ision. Vendor disclaims all implied warranties including fitness for a
 particular purpose. DO NOT USE FOR DIRECT PHYSICAL MANUFACTURING, AUT
OMATED PRODUCTION, OR SAFETY-CRITICAL SYSTEMS without independent engi
neering verification and resolution of any design discrepancies.',(#9039));
#9043=PRODUCT('End Cap Right','End Cap Right',
'LEGAL AND USAGE DISCLAIMER: this Data/Model is provided \X2\201C\X0\A
S IS\X2\201D\X0\ for informational and representational only. It is a 
geometric approximation and is NOT engineered, certified, or guarantee
d for dimensional accuracy, exact tolerances, or production-level prec
ision. Vendor disclaims all implied warranties including fitness for a
 particular purpose. DO NOT USE FOR DIRECT PHYSICAL MANUFACTURING, AUT
OMATED PRODUCTION, OR SAFETY-CRITICAL SYSTEMS without independent engi
neering verification and resolution of any design discrepancies.',(#9039));
#9044=PRODUCT('Z Axis Rod','Z Axis Rod',
'LEGAL AND USAGE DISCLAIMER: this Data/Model is provided \X2\201C\X0\A
S IS\X2\201D\X0\ for informational and representational only. It is a 
geometric approximation and is NOT engineered, certified, or guarantee
d for dimensional accuracy, exact tolerances, or production-level prec
ision. Vendor disclaims all implied warranties including fitness for a
 particular purpose. DO NOT USE FOR DIRECT PHYSICAL MANUFACTURING, AUT
OMATED PRODUCTION, OR SAFETY-CRITICAL SYSTEMS without independent engi
neering verification and resolution of any design discrepancies.',(#9039));
#9045=PRODUCT('Bearing Assembly','Bearing Assembly 1',
'LEGAL AND USAGE DISCLAIMER: this Data/Model is provided \X2\201C\X0\A
S IS\X2\201D\X0\ for informational and representational only. It is a 
geometric approximation and is NOT engineered, certified, or guarantee
d for dimensional accuracy, exact tolerances, or production-level prec
ision. Vendor disclaims all implied warranties including fitness for a
 particular purpose. DO NOT USE FOR DIRECT PHYSICAL MANUFACTURING, AUT
OMATED PRODUCTION, OR SAFETY-CRITICAL SYSTEMS without independent engi
neering verification and resolution of any design discrepancies.',(#9039));
#9046=PRODUCT('Bearing Sleeve','Bearing Sleeve',
'LEGAL AND USAGE DISCLAIMER: this Data/Model is provided \X2\201C\X0\A
S IS\X2\201D\X0\ for informational and representational only. It is a 
geometric approximation and is NOT engineered, certified, or guarantee
d for dimensional accuracy, exact tolerances, or production-level prec
ision. Vendor disclaims all implied warranties including fitness for a
 particular purpose. DO NOT USE FOR DIRECT PHYSICAL MANUFACTURING, AUT
OMATED PRODUCTION, OR SAFETY-CRITICAL SYSTEMS without independent engi
neering verification and resolution of any design discrepancies.',(#9039));
#9047=PRODUCT('Ball Bushing','Ball Bushing',
'LEGAL AND USAGE DISCLAIMER: this Data/Model is provided \X2\201C\X0\A
S IS\X2\201D\X0\ for informational and representational only. It is a 
geometric approximation and is NOT engineered, certified, or guarantee
d for dimensional accuracy, exact tolerances, or production-level prec
ision. Vendor disclaims all implied warranties including fitness for a
 particular purpose. DO NOT USE FOR DIRECT PHYSICAL MANUFACTURING, AUT
OMATED PRODUCTION, OR SAFETY-CRITICAL SYSTEMS without independent engi
neering verification and resolution of any design discrepancies.',(#9039));
#9048=PRODUCT('Bearing Retainer','Bearing Retainer 1',
'LEGAL AND USAGE DISCLAIMER: this Data/Model is provided \X2\201C\X0\A
S IS\X2\201D\X0\ for informational and representational only. It is a 
geometric approximation and is NOT engineered, certified, or guarantee
d for dimensional accuracy, exact tolerances, or production-level prec
ision. Vendor disclaims all implied warranties including fitness for a
 particular purpose. DO NOT USE FOR DIRECT PHYSICAL MANUFACTURING, AUT
OMATED PRODUCTION, OR SAFETY-CRITICAL SYSTEMS without independent engi
neering verification and resolution of any design discrepancies.',(#9039));
#9049=PRODUCT('Gantry Support Bracket','Gantry Support Bracket',
'LEGAL AND USAGE DISCLAIMER: this Data/Model is provided \X2\201C\X0\A
S IS\X2\201D\X0\ for informational and representational only. It is a 
geometric approximation and is NOT engineered, certified, or guarantee
d for dimensional accuracy, exact tolerances, or production-level prec
ision. Vendor disclaims all implied warranties including fitness for a
 particular purpose. DO NOT USE FOR DIRECT PHYSICAL MANUFACTURING, AUT
OMATED PRODUCTION, OR SAFETY-CRITICAL SYSTEMS without independent engi
neering verification and resolution of any design discrepancies.',(#9039));
#9050=PRODUCT('Gantry Carriage Bracket','Gantry Carriage Bracket',
'LEGAL AND USAGE DISCLAIMER: this Data/Model is provided \X2\201C\X0\A
S IS\X2\201D\X0\ for informational and representational only. It is a 
geometric approximation and is NOT engineered, certified, or guarantee
d for dimensional accuracy, exact tolerances, or production-level prec
ision. Vendor disclaims all implied warranties including fitness for a
 particular purpose. DO NOT USE FOR DIRECT PHYSICAL MANUFACTURING, AUT
OMATED PRODUCTION, OR SAFETY-CRITICAL SYSTEMS without independent engi
neering verification and resolution of any design discrepancies.',(#9039));
#9051=PRESENTATION_STYLE_ASSIGNMENT((#9056));
#9052=PRESENTATION_STYLE_ASSIGNMENT((#9057));
#9053=PRESENTATION_STYLE_ASSIGNMENT((#9058));
#9054=PRESENTATION_STYLE_ASSIGNMENT((#9059));
#9055=PRESENTATION_STYLE_ASSIGNMENT((#9060));
#9056=SURFACE_STYLE_USAGE(.BOTH.,#9061);
#9057=SURFACE_STYLE_USAGE(.BOTH.,#9062);
#9058=SURFACE_STYLE_USAGE(.BOTH.,#9063);
#9059=SURFACE_STYLE_USAGE(.BOTH.,#9064);
#9060=SURFACE_STYLE_USAGE(.BOTH.,#9065);
#9061=SURFACE_SIDE_STYLE('',(#9066));
#9062=SURFACE_SIDE_STYLE('',(#9067));
#9063=SURFACE_SIDE_STYLE('',(#9068));
#9064=SURFACE_SIDE_STYLE('',(#9069));
#9065=SURFACE_SIDE_STYLE('',(#9070));
#9066=SURFACE_STYLE_FILL_AREA(#9071);
#9067=SURFACE_STYLE_FILL_AREA(#9072);
#9068=SURFACE_STYLE_FILL_AREA(#9073);
#9069=SURFACE_STYLE_FILL_AREA(#9074);
#9070=SURFACE_STYLE_FILL_AREA(#9075);
#9071=FILL_AREA_STYLE('Steel - Satin',(#9076));
#9072=FILL_AREA_STYLE('Opaque(25,25,25)',(#9077));
#9073=FILL_AREA_STYLE('Opaque(89,149,218)',(#9078));
#9074=FILL_AREA_STYLE('Opaque(137,137,137)',(#9079));
#9075=FILL_AREA_STYLE('Opaque(48,59,150)',(#9080));
#9076=FILL_AREA_STYLE_COLOUR('Steel - Satin',#9081);
#9077=FILL_AREA_STYLE_COLOUR('Opaque(25,25,25)',#9082);
#9078=FILL_AREA_STYLE_COLOUR('Opaque(89,149,218)',#9083);
#9079=FILL_AREA_STYLE_COLOUR('Opaque(137,137,137)',#9084);
#9080=FILL_AREA_STYLE_COLOUR('Opaque(48,59,150)',#9085);
#9081=COLOUR_RGB('Steel - Satin',0.627450980392157,0.627450980392157,0.627450980392157);
#9082=COLOUR_RGB('Opaque(25,25,25)',0.0980392156862745,0.0980392156862745,
0.0980392156862745);
#9083=COLOUR_RGB('Opaque(89,149,218)',0.349019607843137,0.584313725490196,
0.854901960784314);
#9084=COLOUR_RGB('Opaque(137,137,137)',0.537254901960784,0.537254901960784,
0.537254901960784);
#9085=COLOUR_RGB('Opaque(48,59,150)',0.188235294117647,0.231372549019608,
0.588235294117647);
ENDSEC;
END-ISO-10303-21;
